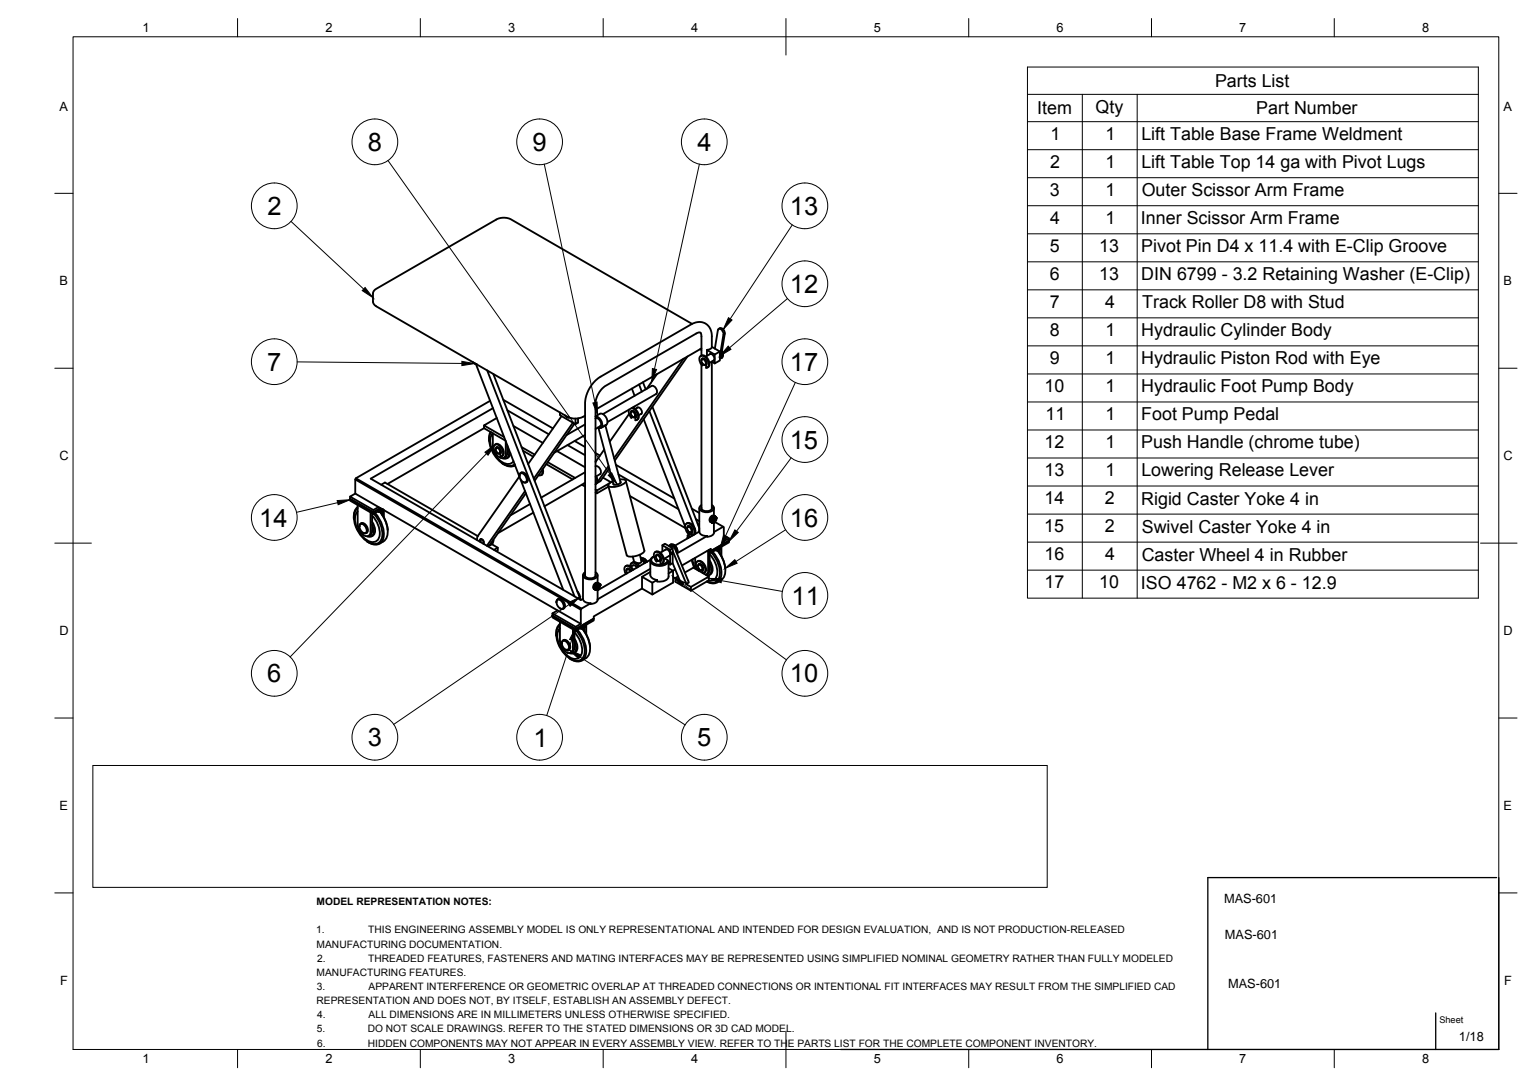
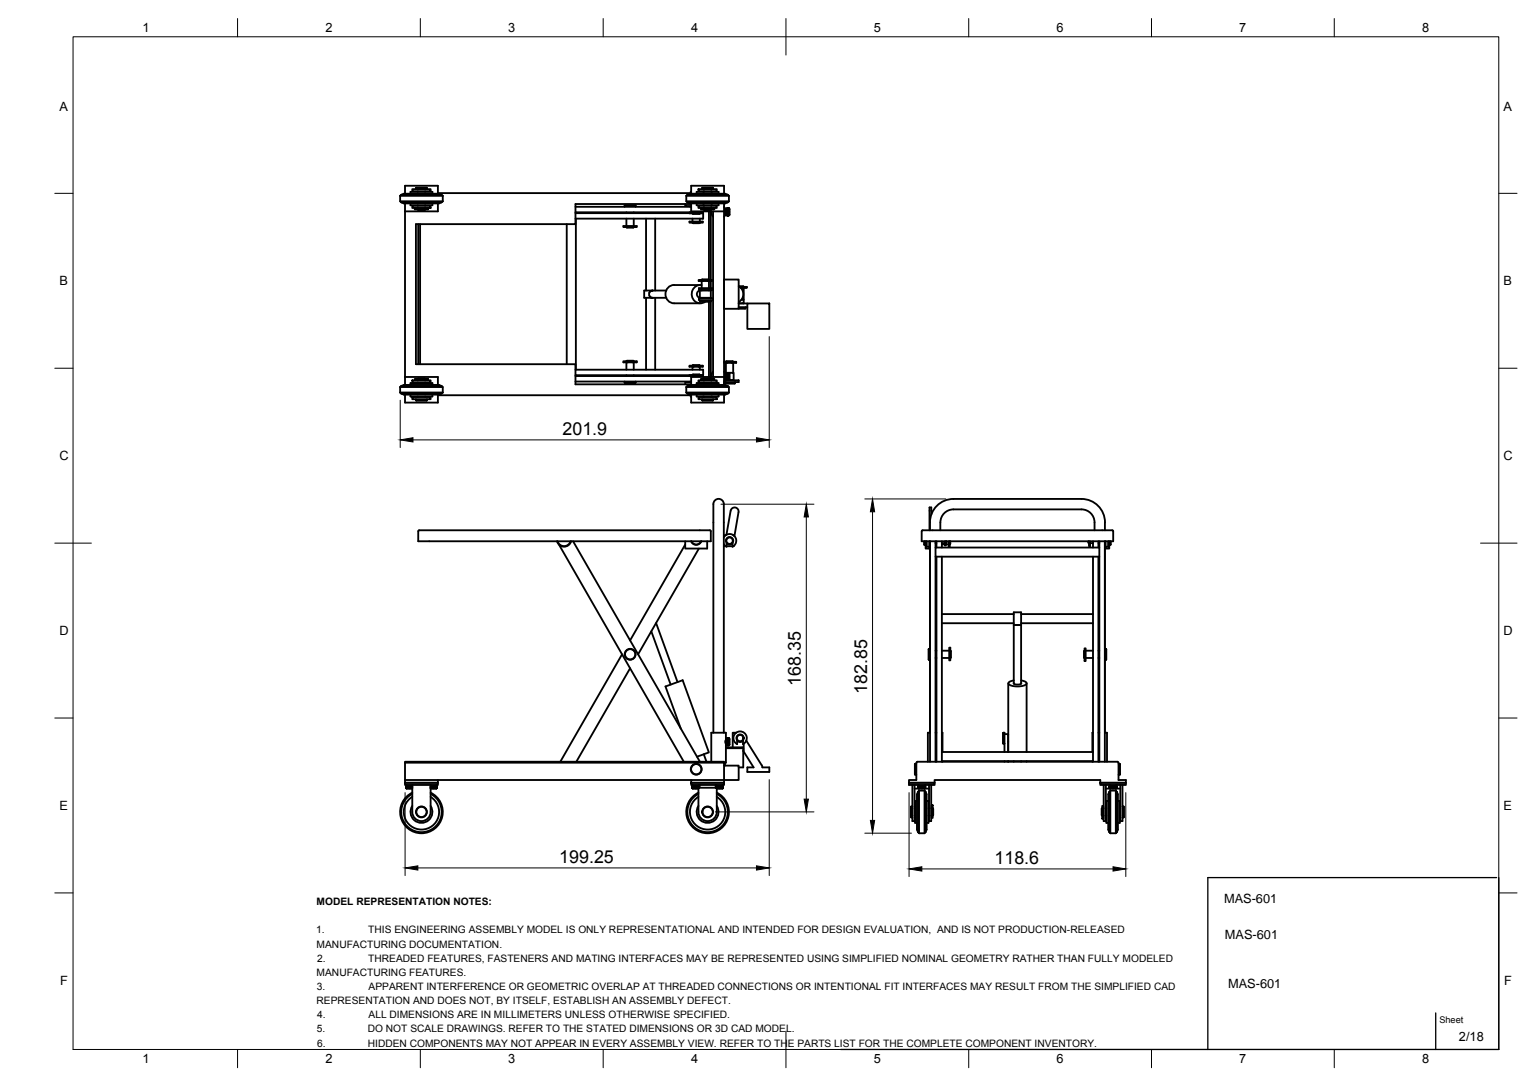
ISO-10303-21;
HEADER;
FILE_DESCRIPTION((''),'2;1');
FILE_NAME('MAS-601','2026-10-06T07:37:42+05:00',(''),(''),'','','');
FILE_SCHEMA (('AUTOMOTIVE_DESIGN { 1 0 10303 214 3 1 1 }'));
ENDSEC;
DATA;
#10 = MECHANICAL_DESIGN_GEOMETRIC_PRESENTATION_REPRESENTATION('',(#373,#374,
#375,#376,#377,#378,#379,#380,#381,#382,#383,#384,#385,#386,#387,#388,#389),
#18757) ;
#11 = ITEM_DEFINED_TRANSFORMATION($,$,#9748,#10657) ;
#12 = ITEM_DEFINED_TRANSFORMATION($,$,#9905,#10658) ;
#13 = ITEM_DEFINED_TRANSFORMATION($,$,#9983,#10659) ;
#14 = ITEM_DEFINED_TRANSFORMATION($,$,#10025,#10660) ;
#15 = ITEM_DEFINED_TRANSFORMATION($,$,#10219,#10661) ;
#16 = ITEM_DEFINED_TRANSFORMATION($,$,#10241,#10662) ;
#17 = ITEM_DEFINED_TRANSFORMATION($,$,#10254,#10663) ;
#18 = ITEM_DEFINED_TRANSFORMATION($,$,#10070,#10664) ;
#19 = ITEM_DEFINED_TRANSFORMATION($,$,#10098,#10665) ;
#20 = ITEM_DEFINED_TRANSFORMATION($,$,#10122,#10666) ;
#21 = ITEM_DEFINED_TRANSFORMATION($,$,#10152,#10667) ;
#22 = ITEM_DEFINED_TRANSFORMATION($,$,#10171,#10668) ;
#23 = ITEM_DEFINED_TRANSFORMATION($,$,#10205,#10669) ;
#24 = ITEM_DEFINED_TRANSFORMATION($,$,#10599,#10670) ;
#25 = ITEM_DEFINED_TRANSFORMATION($,$,#10552,#10671) ;
#26 = ITEM_DEFINED_TRANSFORMATION($,$,#10632,#10672) ;
#27 = ITEM_DEFINED_TRANSFORMATION($,$,#10270,#10673) ;
#28 = ITEM_DEFINED_TRANSFORMATION($,$,#10219,#10674) ;
#29 = ITEM_DEFINED_TRANSFORMATION($,$,#10241,#10675) ;
#30 = ITEM_DEFINED_TRANSFORMATION($,$,#10219,#10676) ;
#31 = ITEM_DEFINED_TRANSFORMATION($,$,#10241,#10677) ;
#32 = ITEM_DEFINED_TRANSFORMATION($,$,#10219,#10678) ;
#33 = ITEM_DEFINED_TRANSFORMATION($,$,#10241,#10679) ;
#34 = ITEM_DEFINED_TRANSFORMATION($,$,#10219,#10680) ;
#35 = ITEM_DEFINED_TRANSFORMATION($,$,#10241,#10681) ;
#36 = ITEM_DEFINED_TRANSFORMATION($,$,#10219,#10682) ;
#37 = ITEM_DEFINED_TRANSFORMATION($,$,#10241,#10683) ;
#38 = ITEM_DEFINED_TRANSFORMATION($,$,#10219,#10684) ;
#39 = ITEM_DEFINED_TRANSFORMATION($,$,#10241,#10685) ;
#40 = ITEM_DEFINED_TRANSFORMATION($,$,#10219,#10686) ;
#41 = ITEM_DEFINED_TRANSFORMATION($,$,#10241,#10687) ;
#42 = ITEM_DEFINED_TRANSFORMATION($,$,#10219,#10688) ;
#43 = ITEM_DEFINED_TRANSFORMATION($,$,#10241,#10689) ;
#44 = ITEM_DEFINED_TRANSFORMATION($,$,#10219,#10690) ;
#45 = ITEM_DEFINED_TRANSFORMATION($,$,#10241,#10691) ;
#46 = ITEM_DEFINED_TRANSFORMATION($,$,#10219,#10692) ;
#47 = ITEM_DEFINED_TRANSFORMATION($,$,#10241,#10693) ;
#48 = ITEM_DEFINED_TRANSFORMATION($,$,#10219,#10694) ;
#49 = ITEM_DEFINED_TRANSFORMATION($,$,#10241,#10695) ;
#50 = ITEM_DEFINED_TRANSFORMATION($,$,#10219,#10696) ;
#51 = ITEM_DEFINED_TRANSFORMATION($,$,#10241,#10697) ;
#52 = ITEM_DEFINED_TRANSFORMATION($,$,#10254,#10698) ;
#53 = ITEM_DEFINED_TRANSFORMATION($,$,#10254,#10699) ;
#54 = ITEM_DEFINED_TRANSFORMATION($,$,#10254,#10700) ;
#55 = ITEM_DEFINED_TRANSFORMATION($,$,#10270,#10701) ;
#56 = ITEM_DEFINED_TRANSFORMATION($,$,#10270,#10702) ;
#57 = ITEM_DEFINED_TRANSFORMATION($,$,#10270,#10703) ;
#58 = ITEM_DEFINED_TRANSFORMATION($,$,#10270,#10704) ;
#59 = ITEM_DEFINED_TRANSFORMATION($,$,#10270,#10705) ;
#60 = ITEM_DEFINED_TRANSFORMATION($,$,#10270,#10706) ;
#61 = ITEM_DEFINED_TRANSFORMATION($,$,#10270,#10707) ;
#62 = ITEM_DEFINED_TRANSFORMATION($,$,#10270,#10708) ;
#63 = ITEM_DEFINED_TRANSFORMATION($,$,#10270,#10709) ;
#64 = ITEM_DEFINED_TRANSFORMATION($,$,#10552,#10710) ;
#65 = ITEM_DEFINED_TRANSFORMATION($,$,#10599,#10711) ;
#66 = ITEM_DEFINED_TRANSFORMATION($,$,#10632,#10712) ;
#67 = ITEM_DEFINED_TRANSFORMATION($,$,#10632,#10713) ;
#68 = ITEM_DEFINED_TRANSFORMATION($,$,#10632,#10714) ;
#69 = (
REPRESENTATION_RELATIONSHIP($,$,#18857,#18856)
REPRESENTATION_RELATIONSHIP_WITH_TRANSFORMATION(#11)
SHAPE_REPRESENTATION_RELATIONSHIP()
) ;
#70 = (
REPRESENTATION_RELATIONSHIP($,$,#18858,#18856)
REPRESENTATION_RELATIONSHIP_WITH_TRANSFORMATION(#12)
SHAPE_REPRESENTATION_RELATIONSHIP()
) ;
#71 = (
REPRESENTATION_RELATIONSHIP($,$,#18859,#18856)
REPRESENTATION_RELATIONSHIP_WITH_TRANSFORMATION(#13)
SHAPE_REPRESENTATION_RELATIONSHIP()
) ;
#72 = (
REPRESENTATION_RELATIONSHIP($,$,#18860,#18856)
REPRESENTATION_RELATIONSHIP_WITH_TRANSFORMATION(#14)
SHAPE_REPRESENTATION_RELATIONSHIP()
) ;
#73 = (
REPRESENTATION_RELATIONSHIP($,$,#18867,#18856)
REPRESENTATION_RELATIONSHIP_WITH_TRANSFORMATION(#15)
SHAPE_REPRESENTATION_RELATIONSHIP()
) ;
#74 = (
REPRESENTATION_RELATIONSHIP($,$,#18868,#18856)
REPRESENTATION_RELATIONSHIP_WITH_TRANSFORMATION(#16)
SHAPE_REPRESENTATION_RELATIONSHIP()
) ;
#75 = (
REPRESENTATION_RELATIONSHIP($,$,#18869,#18856)
REPRESENTATION_RELATIONSHIP_WITH_TRANSFORMATION(#17)
SHAPE_REPRESENTATION_RELATIONSHIP()
) ;
#76 = (
REPRESENTATION_RELATIONSHIP($,$,#18861,#18856)
REPRESENTATION_RELATIONSHIP_WITH_TRANSFORMATION(#18)
SHAPE_REPRESENTATION_RELATIONSHIP()
) ;
#77 = (
REPRESENTATION_RELATIONSHIP($,$,#18862,#18856)
REPRESENTATION_RELATIONSHIP_WITH_TRANSFORMATION(#19)
SHAPE_REPRESENTATION_RELATIONSHIP()
) ;
#78 = (
REPRESENTATION_RELATIONSHIP($,$,#18863,#18856)
REPRESENTATION_RELATIONSHIP_WITH_TRANSFORMATION(#20)
SHAPE_REPRESENTATION_RELATIONSHIP()
) ;
#79 = (
REPRESENTATION_RELATIONSHIP($,$,#18864,#18856)
REPRESENTATION_RELATIONSHIP_WITH_TRANSFORMATION(#21)
SHAPE_REPRESENTATION_RELATIONSHIP()
) ;
#80 = (
REPRESENTATION_RELATIONSHIP($,$,#18865,#18856)
REPRESENTATION_RELATIONSHIP_WITH_TRANSFORMATION(#22)
SHAPE_REPRESENTATION_RELATIONSHIP()
) ;
#81 = (
REPRESENTATION_RELATIONSHIP($,$,#18866,#18856)
REPRESENTATION_RELATIONSHIP_WITH_TRANSFORMATION(#23)
SHAPE_REPRESENTATION_RELATIONSHIP()
) ;
#82 = (
REPRESENTATION_RELATIONSHIP($,$,#18872,#18856)
REPRESENTATION_RELATIONSHIP_WITH_TRANSFORMATION(#24)
SHAPE_REPRESENTATION_RELATIONSHIP()
) ;
#83 = (
REPRESENTATION_RELATIONSHIP($,$,#18871,#18856)
REPRESENTATION_RELATIONSHIP_WITH_TRANSFORMATION(#25)
SHAPE_REPRESENTATION_RELATIONSHIP()
) ;
#84 = (
REPRESENTATION_RELATIONSHIP($,$,#18873,#18856)
REPRESENTATION_RELATIONSHIP_WITH_TRANSFORMATION(#26)
SHAPE_REPRESENTATION_RELATIONSHIP()
) ;
#85 = (
REPRESENTATION_RELATIONSHIP($,$,#18870,#18856)
REPRESENTATION_RELATIONSHIP_WITH_TRANSFORMATION(#27)
SHAPE_REPRESENTATION_RELATIONSHIP()
) ;
#86 = (
REPRESENTATION_RELATIONSHIP($,$,#18867,#18856)
REPRESENTATION_RELATIONSHIP_WITH_TRANSFORMATION(#28)
SHAPE_REPRESENTATION_RELATIONSHIP()
) ;
#87 = (
REPRESENTATION_RELATIONSHIP($,$,#18868,#18856)
REPRESENTATION_RELATIONSHIP_WITH_TRANSFORMATION(#29)
SHAPE_REPRESENTATION_RELATIONSHIP()
) ;
#88 = (
REPRESENTATION_RELATIONSHIP($,$,#18867,#18856)
REPRESENTATION_RELATIONSHIP_WITH_TRANSFORMATION(#30)
SHAPE_REPRESENTATION_RELATIONSHIP()
) ;
#89 = (
REPRESENTATION_RELATIONSHIP($,$,#18868,#18856)
REPRESENTATION_RELATIONSHIP_WITH_TRANSFORMATION(#31)
SHAPE_REPRESENTATION_RELATIONSHIP()
) ;
#90 = (
REPRESENTATION_RELATIONSHIP($,$,#18867,#18856)
REPRESENTATION_RELATIONSHIP_WITH_TRANSFORMATION(#32)
SHAPE_REPRESENTATION_RELATIONSHIP()
) ;
#91 = (
REPRESENTATION_RELATIONSHIP($,$,#18868,#18856)
REPRESENTATION_RELATIONSHIP_WITH_TRANSFORMATION(#33)
SHAPE_REPRESENTATION_RELATIONSHIP()
) ;
#92 = (
REPRESENTATION_RELATIONSHIP($,$,#18867,#18856)
REPRESENTATION_RELATIONSHIP_WITH_TRANSFORMATION(#34)
SHAPE_REPRESENTATION_RELATIONSHIP()
) ;
#93 = (
REPRESENTATION_RELATIONSHIP($,$,#18868,#18856)
REPRESENTATION_RELATIONSHIP_WITH_TRANSFORMATION(#35)
SHAPE_REPRESENTATION_RELATIONSHIP()
) ;
#94 = (
REPRESENTATION_RELATIONSHIP($,$,#18867,#18856)
REPRESENTATION_RELATIONSHIP_WITH_TRANSFORMATION(#36)
SHAPE_REPRESENTATION_RELATIONSHIP()
) ;
#95 = (
REPRESENTATION_RELATIONSHIP($,$,#18868,#18856)
REPRESENTATION_RELATIONSHIP_WITH_TRANSFORMATION(#37)
SHAPE_REPRESENTATION_RELATIONSHIP()
) ;
#96 = (
REPRESENTATION_RELATIONSHIP($,$,#18867,#18856)
REPRESENTATION_RELATIONSHIP_WITH_TRANSFORMATION(#38)
SHAPE_REPRESENTATION_RELATIONSHIP()
) ;
#97 = (
REPRESENTATION_RELATIONSHIP($,$,#18868,#18856)
REPRESENTATION_RELATIONSHIP_WITH_TRANSFORMATION(#39)
SHAPE_REPRESENTATION_RELATIONSHIP()
) ;
#98 = (
REPRESENTATION_RELATIONSHIP($,$,#18867,#18856)
REPRESENTATION_RELATIONSHIP_WITH_TRANSFORMATION(#40)
SHAPE_REPRESENTATION_RELATIONSHIP()
) ;
#99 = (
REPRESENTATION_RELATIONSHIP($,$,#18868,#18856)
REPRESENTATION_RELATIONSHIP_WITH_TRANSFORMATION(#41)
SHAPE_REPRESENTATION_RELATIONSHIP()
) ;
#100 = (
REPRESENTATION_RELATIONSHIP($,$,#18867,#18856)
REPRESENTATION_RELATIONSHIP_WITH_TRANSFORMATION(#42)
SHAPE_REPRESENTATION_RELATIONSHIP()
) ;
#101 = (
REPRESENTATION_RELATIONSHIP($,$,#18868,#18856)
REPRESENTATION_RELATIONSHIP_WITH_TRANSFORMATION(#43)
SHAPE_REPRESENTATION_RELATIONSHIP()
) ;
#102 = (
REPRESENTATION_RELATIONSHIP($,$,#18867,#18856)
REPRESENTATION_RELATIONSHIP_WITH_TRANSFORMATION(#44)
SHAPE_REPRESENTATION_RELATIONSHIP()
) ;
#103 = (
REPRESENTATION_RELATIONSHIP($,$,#18868,#18856)
REPRESENTATION_RELATIONSHIP_WITH_TRANSFORMATION(#45)
SHAPE_REPRESENTATION_RELATIONSHIP()
) ;
#104 = (
REPRESENTATION_RELATIONSHIP($,$,#18867,#18856)
REPRESENTATION_RELATIONSHIP_WITH_TRANSFORMATION(#46)
SHAPE_REPRESENTATION_RELATIONSHIP()
) ;
#105 = (
REPRESENTATION_RELATIONSHIP($,$,#18868,#18856)
REPRESENTATION_RELATIONSHIP_WITH_TRANSFORMATION(#47)
SHAPE_REPRESENTATION_RELATIONSHIP()
) ;
#106 = (
REPRESENTATION_RELATIONSHIP($,$,#18867,#18856)
REPRESENTATION_RELATIONSHIP_WITH_TRANSFORMATION(#48)
SHAPE_REPRESENTATION_RELATIONSHIP()
) ;
#107 = (
REPRESENTATION_RELATIONSHIP($,$,#18868,#18856)
REPRESENTATION_RELATIONSHIP_WITH_TRANSFORMATION(#49)
SHAPE_REPRESENTATION_RELATIONSHIP()
) ;
#108 = (
REPRESENTATION_RELATIONSHIP($,$,#18867,#18856)
REPRESENTATION_RELATIONSHIP_WITH_TRANSFORMATION(#50)
SHAPE_REPRESENTATION_RELATIONSHIP()
) ;
#109 = (
REPRESENTATION_RELATIONSHIP($,$,#18868,#18856)
REPRESENTATION_RELATIONSHIP_WITH_TRANSFORMATION(#51)
SHAPE_REPRESENTATION_RELATIONSHIP()
) ;
#110 = (
REPRESENTATION_RELATIONSHIP($,$,#18869,#18856)
REPRESENTATION_RELATIONSHIP_WITH_TRANSFORMATION(#52)
SHAPE_REPRESENTATION_RELATIONSHIP()
) ;
#111 = (
REPRESENTATION_RELATIONSHIP($,$,#18869,#18856)
REPRESENTATION_RELATIONSHIP_WITH_TRANSFORMATION(#53)
SHAPE_REPRESENTATION_RELATIONSHIP()
) ;
#112 = (
REPRESENTATION_RELATIONSHIP($,$,#18869,#18856)
REPRESENTATION_RELATIONSHIP_WITH_TRANSFORMATION(#54)
SHAPE_REPRESENTATION_RELATIONSHIP()
) ;
#113 = (
REPRESENTATION_RELATIONSHIP($,$,#18870,#18856)
REPRESENTATION_RELATIONSHIP_WITH_TRANSFORMATION(#55)
SHAPE_REPRESENTATION_RELATIONSHIP()
) ;
#114 = (
REPRESENTATION_RELATIONSHIP($,$,#18870,#18856)
REPRESENTATION_RELATIONSHIP_WITH_TRANSFORMATION(#56)
SHAPE_REPRESENTATION_RELATIONSHIP()
) ;
#115 = (
REPRESENTATION_RELATIONSHIP($,$,#18870,#18856)
REPRESENTATION_RELATIONSHIP_WITH_TRANSFORMATION(#57)
SHAPE_REPRESENTATION_RELATIONSHIP()
) ;
#116 = (
REPRESENTATION_RELATIONSHIP($,$,#18870,#18856)
REPRESENTATION_RELATIONSHIP_WITH_TRANSFORMATION(#58)
SHAPE_REPRESENTATION_RELATIONSHIP()
) ;
#117 = (
REPRESENTATION_RELATIONSHIP($,$,#18870,#18856)
REPRESENTATION_RELATIONSHIP_WITH_TRANSFORMATION(#59)
SHAPE_REPRESENTATION_RELATIONSHIP()
) ;
#118 = (
REPRESENTATION_RELATIONSHIP($,$,#18870,#18856)
REPRESENTATION_RELATIONSHIP_WITH_TRANSFORMATION(#60)
SHAPE_REPRESENTATION_RELATIONSHIP()
) ;
#119 = (
REPRESENTATION_RELATIONSHIP($,$,#18870,#18856)
REPRESENTATION_RELATIONSHIP_WITH_TRANSFORMATION(#61)
SHAPE_REPRESENTATION_RELATIONSHIP()
) ;
#120 = (
REPRESENTATION_RELATIONSHIP($,$,#18870,#18856)
REPRESENTATION_RELATIONSHIP_WITH_TRANSFORMATION(#62)
SHAPE_REPRESENTATION_RELATIONSHIP()
) ;
#121 = (
REPRESENTATION_RELATIONSHIP($,$,#18870,#18856)
REPRESENTATION_RELATIONSHIP_WITH_TRANSFORMATION(#63)
SHAPE_REPRESENTATION_RELATIONSHIP()
) ;
#122 = (
REPRESENTATION_RELATIONSHIP($,$,#18871,#18856)
REPRESENTATION_RELATIONSHIP_WITH_TRANSFORMATION(#64)
SHAPE_REPRESENTATION_RELATIONSHIP()
) ;
#123 = (
REPRESENTATION_RELATIONSHIP($,$,#18872,#18856)
REPRESENTATION_RELATIONSHIP_WITH_TRANSFORMATION(#65)
SHAPE_REPRESENTATION_RELATIONSHIP()
) ;
#124 = (
REPRESENTATION_RELATIONSHIP($,$,#18873,#18856)
REPRESENTATION_RELATIONSHIP_WITH_TRANSFORMATION(#66)
SHAPE_REPRESENTATION_RELATIONSHIP()
) ;
#125 = (
REPRESENTATION_RELATIONSHIP($,$,#18873,#18856)
REPRESENTATION_RELATIONSHIP_WITH_TRANSFORMATION(#67)
SHAPE_REPRESENTATION_RELATIONSHIP()
) ;
#126 = (
REPRESENTATION_RELATIONSHIP($,$,#18873,#18856)
REPRESENTATION_RELATIONSHIP_WITH_TRANSFORMATION(#68)
SHAPE_REPRESENTATION_RELATIONSHIP()
) ;
#127 = CONTEXT_DEPENDENT_SHAPE_REPRESENTATION(#69,#18798) ;
#128 = CONTEXT_DEPENDENT_SHAPE_REPRESENTATION(#70,#18799) ;
#129 = CONTEXT_DEPENDENT_SHAPE_REPRESENTATION(#71,#18800) ;
#130 = CONTEXT_DEPENDENT_SHAPE_REPRESENTATION(#72,#18801) ;
#131 = CONTEXT_DEPENDENT_SHAPE_REPRESENTATION(#73,#18802) ;
#132 = CONTEXT_DEPENDENT_SHAPE_REPRESENTATION(#74,#18803) ;
#133 = CONTEXT_DEPENDENT_SHAPE_REPRESENTATION(#75,#18804) ;
#134 = CONTEXT_DEPENDENT_SHAPE_REPRESENTATION(#76,#18805) ;
#135 = CONTEXT_DEPENDENT_SHAPE_REPRESENTATION(#77,#18806) ;
#136 = CONTEXT_DEPENDENT_SHAPE_REPRESENTATION(#78,#18807) ;
#137 = CONTEXT_DEPENDENT_SHAPE_REPRESENTATION(#79,#18808) ;
#138 = CONTEXT_DEPENDENT_SHAPE_REPRESENTATION(#80,#18809) ;
#139 = CONTEXT_DEPENDENT_SHAPE_REPRESENTATION(#81,#18810) ;
#140 = CONTEXT_DEPENDENT_SHAPE_REPRESENTATION(#82,#18811) ;
#141 = CONTEXT_DEPENDENT_SHAPE_REPRESENTATION(#83,#18812) ;
#142 = CONTEXT_DEPENDENT_SHAPE_REPRESENTATION(#84,#18813) ;
#143 = CONTEXT_DEPENDENT_SHAPE_REPRESENTATION(#85,#18814) ;
#144 = CONTEXT_DEPENDENT_SHAPE_REPRESENTATION(#86,#18815) ;
#145 = CONTEXT_DEPENDENT_SHAPE_REPRESENTATION(#87,#18816) ;
#146 = CONTEXT_DEPENDENT_SHAPE_REPRESENTATION(#88,#18817) ;
#147 = CONTEXT_DEPENDENT_SHAPE_REPRESENTATION(#89,#18818) ;
#148 = CONTEXT_DEPENDENT_SHAPE_REPRESENTATION(#90,#18819) ;
#149 = CONTEXT_DEPENDENT_SHAPE_REPRESENTATION(#91,#18820) ;
#150 = CONTEXT_DEPENDENT_SHAPE_REPRESENTATION(#92,#18821) ;
#151 = CONTEXT_DEPENDENT_SHAPE_REPRESENTATION(#93,#18822) ;
#152 = CONTEXT_DEPENDENT_SHAPE_REPRESENTATION(#94,#18823) ;
#153 = CONTEXT_DEPENDENT_SHAPE_REPRESENTATION(#95,#18824) ;
#154 = CONTEXT_DEPENDENT_SHAPE_REPRESENTATION(#96,#18825) ;
#155 = CONTEXT_DEPENDENT_SHAPE_REPRESENTATION(#97,#18826) ;
#156 = CONTEXT_DEPENDENT_SHAPE_REPRESENTATION(#98,#18827) ;
#157 = CONTEXT_DEPENDENT_SHAPE_REPRESENTATION(#99,#18828) ;
#158 = CONTEXT_DEPENDENT_SHAPE_REPRESENTATION(#100,#18829) ;
#159 = CONTEXT_DEPENDENT_SHAPE_REPRESENTATION(#101,#18830) ;
#160 = CONTEXT_DEPENDENT_SHAPE_REPRESENTATION(#102,#18831) ;
#161 = CONTEXT_DEPENDENT_SHAPE_REPRESENTATION(#103,#18832) ;
#162 = CONTEXT_DEPENDENT_SHAPE_REPRESENTATION(#104,#18833) ;
#163 = CONTEXT_DEPENDENT_SHAPE_REPRESENTATION(#105,#18834) ;
#164 = CONTEXT_DEPENDENT_SHAPE_REPRESENTATION(#106,#18835) ;
#165 = CONTEXT_DEPENDENT_SHAPE_REPRESENTATION(#107,#18836) ;
#166 = CONTEXT_DEPENDENT_SHAPE_REPRESENTATION(#108,#18837) ;
#167 = CONTEXT_DEPENDENT_SHAPE_REPRESENTATION(#109,#18838) ;
#168 = CONTEXT_DEPENDENT_SHAPE_REPRESENTATION(#110,#18839) ;
#169 = CONTEXT_DEPENDENT_SHAPE_REPRESENTATION(#111,#18840) ;
#170 = CONTEXT_DEPENDENT_SHAPE_REPRESENTATION(#112,#18841) ;
#171 = CONTEXT_DEPENDENT_SHAPE_REPRESENTATION(#113,#18842) ;
#172 = CONTEXT_DEPENDENT_SHAPE_REPRESENTATION(#114,#18843) ;
#173 = CONTEXT_DEPENDENT_SHAPE_REPRESENTATION(#115,#18844) ;
#174 = CONTEXT_DEPENDENT_SHAPE_REPRESENTATION(#116,#18845) ;
#175 = CONTEXT_DEPENDENT_SHAPE_REPRESENTATION(#117,#18846) ;
#176 = CONTEXT_DEPENDENT_SHAPE_REPRESENTATION(#118,#18847) ;
#177 = CONTEXT_DEPENDENT_SHAPE_REPRESENTATION(#119,#18848) ;
#178 = CONTEXT_DEPENDENT_SHAPE_REPRESENTATION(#120,#18849) ;
#179 = CONTEXT_DEPENDENT_SHAPE_REPRESENTATION(#121,#18850) ;
#180 = CONTEXT_DEPENDENT_SHAPE_REPRESENTATION(#122,#18851) ;
#181 = CONTEXT_DEPENDENT_SHAPE_REPRESENTATION(#123,#18852) ;
#182 = CONTEXT_DEPENDENT_SHAPE_REPRESENTATION(#124,#18853) ;
#183 = CONTEXT_DEPENDENT_SHAPE_REPRESENTATION(#125,#18854) ;
#184 = CONTEXT_DEPENDENT_SHAPE_REPRESENTATION(#126,#18855) ;
#185 = NEXT_ASSEMBLY_USAGE_OCCURRENCE('Lift Table Base Frame Weldment:1',
'Lift Table Base Frame Weldment:1','Lift Table Base Frame Weldment:1',#18875,
#18876,'Lift Table Base Frame Weldment:1') ;
#186 = NEXT_ASSEMBLY_USAGE_OCCURRENCE(
'Lift Table Top 14 ga with Pivot Lugs:1',
'Lift Table Top 14 ga with Pivot Lugs:1',
'Lift Table Top 14 ga with Pivot Lugs:1',#18875,#18877,
'Lift Table Top 14 ga with Pivot Lugs:1') ;
#187 = NEXT_ASSEMBLY_USAGE_OCCURRENCE('Outer Scissor Arm Frame:1',
'Outer Scissor Arm Frame:1','Outer Scissor Arm Frame:1',#18875,#18878,
'Outer Scissor Arm Frame:1') ;
#188 = NEXT_ASSEMBLY_USAGE_OCCURRENCE('Inner Scissor Arm Frame:1',
'Inner Scissor Arm Frame:1','Inner Scissor Arm Frame:1',#18875,#18879,
'Inner Scissor Arm Frame:1') ;
#189 = NEXT_ASSEMBLY_USAGE_OCCURRENCE(
'Pivot Pin D4 x 11.4 with E-Clip Groove:1',
'Pivot Pin D4 x 11.4 with E-Clip Groove:1',
'Pivot Pin D4 x 11.4 with E-Clip Groove:1',#18875,#18886,
'Pivot Pin D4 x 11.4 with E-Clip Groove:1') ;
#190 = NEXT_ASSEMBLY_USAGE_OCCURRENCE(
'DIN 6799 - 3.2 Retaining Washer (E-Clip):1',
'DIN 6799 - 3.2 Retaining Washer (E-Clip):1',
'DIN 6799 - 3.2 Retaining Washer (E-Clip):1',#18875,#18887,
'DIN 6799 - 3.2 Retaining Washer (E-Clip):1') ;
#191 = NEXT_ASSEMBLY_USAGE_OCCURRENCE('Track Roller D8 with Stud:1',
'Track Roller D8 with Stud:1','Track Roller D8 with Stud:1',#18875,#18888,
'Track Roller D8 with Stud:1') ;
#192 = NEXT_ASSEMBLY_USAGE_OCCURRENCE('Hydraulic Cylinder Body:1',
'Hydraulic Cylinder Body:1','Hydraulic Cylinder Body:1',#18875,#18880,
'Hydraulic Cylinder Body:1') ;
#193 = NEXT_ASSEMBLY_USAGE_OCCURRENCE('Hydraulic Piston Rod with Eye:1',
'Hydraulic Piston Rod with Eye:1','Hydraulic Piston Rod with Eye:1',#18875,
#18881,'Hydraulic Piston Rod with Eye:1') ;
#194 = NEXT_ASSEMBLY_USAGE_OCCURRENCE('Hydraulic Foot Pump Body:1',
'Hydraulic Foot Pump Body:1','Hydraulic Foot Pump Body:1',#18875,#18882,
'Hydraulic Foot Pump Body:1') ;
#195 = NEXT_ASSEMBLY_USAGE_OCCURRENCE('Foot Pump Pedal:1',
'Foot Pump Pedal:1','Foot Pump Pedal:1',#18875,#18883,
'Foot Pump Pedal:1') ;
#196 = NEXT_ASSEMBLY_USAGE_OCCURRENCE('Push Handle (chrome tube):1',
'Push Handle (chrome tube):1','Push Handle (chrome tube):1',#18875,#18884,
'Push Handle (chrome tube):1') ;
#197 = NEXT_ASSEMBLY_USAGE_OCCURRENCE('Lowering Release Lever:1',
'Lowering Release Lever:1','Lowering Release Lever:1',#18875,#18885,
'Lowering Release Lever:1') ;
#198 = NEXT_ASSEMBLY_USAGE_OCCURRENCE('Rigid Caster Yoke 4 in:1',
'Rigid Caster Yoke 4 in:1','Rigid Caster Yoke 4 in:1',#18875,#18891,
'Rigid Caster Yoke 4 in:1') ;
#199 = NEXT_ASSEMBLY_USAGE_OCCURRENCE('Swivel Caster Yoke 4 in:1',
'Swivel Caster Yoke 4 in:1','Swivel Caster Yoke 4 in:1',#18875,#18890,
'Swivel Caster Yoke 4 in:1') ;
#200 = NEXT_ASSEMBLY_USAGE_OCCURRENCE('Caster Wheel 4 in Rubber:1',
'Caster Wheel 4 in Rubber:1','Caster Wheel 4 in Rubber:1',#18875,#18892,
'Caster Wheel 4 in Rubber:1') ;
#201 = NEXT_ASSEMBLY_USAGE_OCCURRENCE('ISO 4762 - M2 x 6 - 12.9:1',
'ISO 4762 - M2 x 6 - 12.9:1','ISO 4762 - M2 x 6 - 12.9:1',#18875,#18889,
'ISO 4762 - M2 x 6 - 12.9:1') ;
#202 = NEXT_ASSEMBLY_USAGE_OCCURRENCE(
'Pivot Pin D4 x 11.4 with E-Clip Groove:2',
'Pivot Pin D4 x 11.4 with E-Clip Groove:2',
'Pivot Pin D4 x 11.4 with E-Clip Groove:2',#18875,#18886,
'Pivot Pin D4 x 11.4 with E-Clip Groove:2') ;
#203 = NEXT_ASSEMBLY_USAGE_OCCURRENCE(
'DIN 6799 - 3.2 Retaining Washer (E-Clip):2',
'DIN 6799 - 3.2 Retaining Washer (E-Clip):2',
'DIN 6799 - 3.2 Retaining Washer (E-Clip):2',#18875,#18887,
'DIN 6799 - 3.2 Retaining Washer (E-Clip):2') ;
#204 = NEXT_ASSEMBLY_USAGE_OCCURRENCE(
'Pivot Pin D4 x 11.4 with E-Clip Groove:3',
'Pivot Pin D4 x 11.4 with E-Clip Groove:3',
'Pivot Pin D4 x 11.4 with E-Clip Groove:3',#18875,#18886,
'Pivot Pin D4 x 11.4 with E-Clip Groove:3') ;
#205 = NEXT_ASSEMBLY_USAGE_OCCURRENCE(
'DIN 6799 - 3.2 Retaining Washer (E-Clip):3',
'DIN 6799 - 3.2 Retaining Washer (E-Clip):3',
'DIN 6799 - 3.2 Retaining Washer (E-Clip):3',#18875,#18887,
'DIN 6799 - 3.2 Retaining Washer (E-Clip):3') ;
#206 = NEXT_ASSEMBLY_USAGE_OCCURRENCE(
'Pivot Pin D4 x 11.4 with E-Clip Groove:4',
'Pivot Pin D4 x 11.4 with E-Clip Groove:4',
'Pivot Pin D4 x 11.4 with E-Clip Groove:4',#18875,#18886,
'Pivot Pin D4 x 11.4 with E-Clip Groove:4') ;
#207 = NEXT_ASSEMBLY_USAGE_OCCURRENCE(
'DIN 6799 - 3.2 Retaining Washer (E-Clip):4',
'DIN 6799 - 3.2 Retaining Washer (E-Clip):4',
'DIN 6799 - 3.2 Retaining Washer (E-Clip):4',#18875,#18887,
'DIN 6799 - 3.2 Retaining Washer (E-Clip):4') ;
#208 = NEXT_ASSEMBLY_USAGE_OCCURRENCE(
'Pivot Pin D4 x 11.4 with E-Clip Groove:5',
'Pivot Pin D4 x 11.4 with E-Clip Groove:5',
'Pivot Pin D4 x 11.4 with E-Clip Groove:5',#18875,#18886,
'Pivot Pin D4 x 11.4 with E-Clip Groove:5') ;
#209 = NEXT_ASSEMBLY_USAGE_OCCURRENCE(
'DIN 6799 - 3.2 Retaining Washer (E-Clip):5',
'DIN 6799 - 3.2 Retaining Washer (E-Clip):5',
'DIN 6799 - 3.2 Retaining Washer (E-Clip):5',#18875,#18887,
'DIN 6799 - 3.2 Retaining Washer (E-Clip):5') ;
#210 = NEXT_ASSEMBLY_USAGE_OCCURRENCE(
'Pivot Pin D4 x 11.4 with E-Clip Groove:6',
'Pivot Pin D4 x 11.4 with E-Clip Groove:6',
'Pivot Pin D4 x 11.4 with E-Clip Groove:6',#18875,#18886,
'Pivot Pin D4 x 11.4 with E-Clip Groove:6') ;
#211 = NEXT_ASSEMBLY_USAGE_OCCURRENCE(
'DIN 6799 - 3.2 Retaining Washer (E-Clip):6',
'DIN 6799 - 3.2 Retaining Washer (E-Clip):6',
'DIN 6799 - 3.2 Retaining Washer (E-Clip):6',#18875,#18887,
'DIN 6799 - 3.2 Retaining Washer (E-Clip):6') ;
#212 = NEXT_ASSEMBLY_USAGE_OCCURRENCE(
'Pivot Pin D4 x 11.4 with E-Clip Groove:7',
'Pivot Pin D4 x 11.4 with E-Clip Groove:7',
'Pivot Pin D4 x 11.4 with E-Clip Groove:7',#18875,#18886,
'Pivot Pin D4 x 11.4 with E-Clip Groove:7') ;
#213 = NEXT_ASSEMBLY_USAGE_OCCURRENCE(
'DIN 6799 - 3.2 Retaining Washer (E-Clip):7',
'DIN 6799 - 3.2 Retaining Washer (E-Clip):7',
'DIN 6799 - 3.2 Retaining Washer (E-Clip):7',#18875,#18887,
'DIN 6799 - 3.2 Retaining Washer (E-Clip):7') ;
#214 = NEXT_ASSEMBLY_USAGE_OCCURRENCE(
'Pivot Pin D4 x 11.4 with E-Clip Groove:8',
'Pivot Pin D4 x 11.4 with E-Clip Groove:8',
'Pivot Pin D4 x 11.4 with E-Clip Groove:8',#18875,#18886,
'Pivot Pin D4 x 11.4 with E-Clip Groove:8') ;
#215 = NEXT_ASSEMBLY_USAGE_OCCURRENCE(
'DIN 6799 - 3.2 Retaining Washer (E-Clip):8',
'DIN 6799 - 3.2 Retaining Washer (E-Clip):8',
'DIN 6799 - 3.2 Retaining Washer (E-Clip):8',#18875,#18887,
'DIN 6799 - 3.2 Retaining Washer (E-Clip):8') ;
#216 = NEXT_ASSEMBLY_USAGE_OCCURRENCE(
'Pivot Pin D4 x 11.4 with E-Clip Groove:9',
'Pivot Pin D4 x 11.4 with E-Clip Groove:9',
'Pivot Pin D4 x 11.4 with E-Clip Groove:9',#18875,#18886,
'Pivot Pin D4 x 11.4 with E-Clip Groove:9') ;
#217 = NEXT_ASSEMBLY_USAGE_OCCURRENCE(
'DIN 6799 - 3.2 Retaining Washer (E-Clip):9',
'DIN 6799 - 3.2 Retaining Washer (E-Clip):9',
'DIN 6799 - 3.2 Retaining Washer (E-Clip):9',#18875,#18887,
'DIN 6799 - 3.2 Retaining Washer (E-Clip):9') ;
#218 = NEXT_ASSEMBLY_USAGE_OCCURRENCE(
'Pivot Pin D4 x 11.4 with E-Clip Groove:10',
'Pivot Pin D4 x 11.4 with E-Clip Groove:10',
'Pivot Pin D4 x 11.4 with E-Clip Groove:10',#18875,#18886,
'Pivot Pin D4 x 11.4 with E-Clip Groove:10') ;
#219 = NEXT_ASSEMBLY_USAGE_OCCURRENCE(
'DIN 6799 - 3.2 Retaining Washer (E-Clip):10',
'DIN 6799 - 3.2 Retaining Washer (E-Clip):10',
'DIN 6799 - 3.2 Retaining Washer (E-Clip):10',#18875,#18887,
'DIN 6799 - 3.2 Retaining Washer (E-Clip):10') ;
#220 = NEXT_ASSEMBLY_USAGE_OCCURRENCE(
'Pivot Pin D4 x 11.4 with E-Clip Groove:11',
'Pivot Pin D4 x 11.4 with E-Clip Groove:11',
'Pivot Pin D4 x 11.4 with E-Clip Groove:11',#18875,#18886,
'Pivot Pin D4 x 11.4 with E-Clip Groove:11') ;
#221 = NEXT_ASSEMBLY_USAGE_OCCURRENCE(
'DIN 6799 - 3.2 Retaining Washer (E-Clip):11',
'DIN 6799 - 3.2 Retaining Washer (E-Clip):11',
'DIN 6799 - 3.2 Retaining Washer (E-Clip):11',#18875,#18887,
'DIN 6799 - 3.2 Retaining Washer (E-Clip):11') ;
#222 = NEXT_ASSEMBLY_USAGE_OCCURRENCE(
'Pivot Pin D4 x 11.4 with E-Clip Groove:12',
'Pivot Pin D4 x 11.4 with E-Clip Groove:12',
'Pivot Pin D4 x 11.4 with E-Clip Groove:12',#18875,#18886,
'Pivot Pin D4 x 11.4 with E-Clip Groove:12') ;
#223 = NEXT_ASSEMBLY_USAGE_OCCURRENCE(
'DIN 6799 - 3.2 Retaining Washer (E-Clip):12',
'DIN 6799 - 3.2 Retaining Washer (E-Clip):12',
'DIN 6799 - 3.2 Retaining Washer (E-Clip):12',#18875,#18887,
'DIN 6799 - 3.2 Retaining Washer (E-Clip):12') ;
#224 = NEXT_ASSEMBLY_USAGE_OCCURRENCE(
'Pivot Pin D4 x 11.4 with E-Clip Groove:13',
'Pivot Pin D4 x 11.4 with E-Clip Groove:13',
'Pivot Pin D4 x 11.4 with E-Clip Groove:13',#18875,#18886,
'Pivot Pin D4 x 11.4 with E-Clip Groove:13') ;
#225 = NEXT_ASSEMBLY_USAGE_OCCURRENCE(
'DIN 6799 - 3.2 Retaining Washer (E-Clip):13',
'DIN 6799 - 3.2 Retaining Washer (E-Clip):13',
'DIN 6799 - 3.2 Retaining Washer (E-Clip):13',#18875,#18887,
'DIN 6799 - 3.2 Retaining Washer (E-Clip):13') ;
#226 = NEXT_ASSEMBLY_USAGE_OCCURRENCE('Track Roller D8 with Stud:2',
'Track Roller D8 with Stud:2','Track Roller D8 with Stud:2',#18875,#18888,
'Track Roller D8 with Stud:2') ;
#227 = NEXT_ASSEMBLY_USAGE_OCCURRENCE('Track Roller D8 with Stud:3',
'Track Roller D8 with Stud:3','Track Roller D8 with Stud:3',#18875,#18888,
'Track Roller D8 with Stud:3') ;
#228 = NEXT_ASSEMBLY_USAGE_OCCURRENCE('Track Roller D8 with Stud:4',
'Track Roller D8 with Stud:4','Track Roller D8 with Stud:4',#18875,#18888,
'Track Roller D8 with Stud:4') ;
#229 = NEXT_ASSEMBLY_USAGE_OCCURRENCE('ISO 4762 - M2 x 6 - 12.9:2',
'ISO 4762 - M2 x 6 - 12.9:2','ISO 4762 - M2 x 6 - 12.9:2',#18875,#18889,
'ISO 4762 - M2 x 6 - 12.9:2') ;
#230 = NEXT_ASSEMBLY_USAGE_OCCURRENCE('ISO 4762 - M2 x 6 - 12.9:3',
'ISO 4762 - M2 x 6 - 12.9:3','ISO 4762 - M2 x 6 - 12.9:3',#18875,#18889,
'ISO 4762 - M2 x 6 - 12.9:3') ;
#231 = NEXT_ASSEMBLY_USAGE_OCCURRENCE('ISO 4762 - M2 x 6 - 12.9:4',
'ISO 4762 - M2 x 6 - 12.9:4','ISO 4762 - M2 x 6 - 12.9:4',#18875,#18889,
'ISO 4762 - M2 x 6 - 12.9:4') ;
#232 = NEXT_ASSEMBLY_USAGE_OCCURRENCE('ISO 4762 - M2 x 6 - 12.9:5',
'ISO 4762 - M2 x 6 - 12.9:5','ISO 4762 - M2 x 6 - 12.9:5',#18875,#18889,
'ISO 4762 - M2 x 6 - 12.9:5') ;
#233 = NEXT_ASSEMBLY_USAGE_OCCURRENCE('ISO 4762 - M2 x 6 - 12.9:6',
'ISO 4762 - M2 x 6 - 12.9:6','ISO 4762 - M2 x 6 - 12.9:6',#18875,#18889,
'ISO 4762 - M2 x 6 - 12.9:6') ;
#234 = NEXT_ASSEMBLY_USAGE_OCCURRENCE('ISO 4762 - M2 x 6 - 12.9:7',
'ISO 4762 - M2 x 6 - 12.9:7','ISO 4762 - M2 x 6 - 12.9:7',#18875,#18889,
'ISO 4762 - M2 x 6 - 12.9:7') ;
#235 = NEXT_ASSEMBLY_USAGE_OCCURRENCE('ISO 4762 - M2 x 6 - 12.9:8',
'ISO 4762 - M2 x 6 - 12.9:8','ISO 4762 - M2 x 6 - 12.9:8',#18875,#18889,
'ISO 4762 - M2 x 6 - 12.9:8') ;
#236 = NEXT_ASSEMBLY_USAGE_OCCURRENCE('ISO 4762 - M2 x 6 - 12.9:9',
'ISO 4762 - M2 x 6 - 12.9:9','ISO 4762 - M2 x 6 - 12.9:9',#18875,#18889,
'ISO 4762 - M2 x 6 - 12.9:9') ;
#237 = NEXT_ASSEMBLY_USAGE_OCCURRENCE('ISO 4762 - M2 x 6 - 12.9:10',
'ISO 4762 - M2 x 6 - 12.9:10','ISO 4762 - M2 x 6 - 12.9:10',#18875,#18889,
'ISO 4762 - M2 x 6 - 12.9:10') ;
#238 = NEXT_ASSEMBLY_USAGE_OCCURRENCE('Swivel Caster Yoke 4 in:2',
'Swivel Caster Yoke 4 in:2','Swivel Caster Yoke 4 in:2',#18875,#18890,
'Swivel Caster Yoke 4 in:2') ;
#239 = NEXT_ASSEMBLY_USAGE_OCCURRENCE('Rigid Caster Yoke 4 in:2',
'Rigid Caster Yoke 4 in:2','Rigid Caster Yoke 4 in:2',#18875,#18891,
'Rigid Caster Yoke 4 in:2') ;
#240 = NEXT_ASSEMBLY_USAGE_OCCURRENCE('Caster Wheel 4 in Rubber:2',
'Caster Wheel 4 in Rubber:2','Caster Wheel 4 in Rubber:2',#18875,#18892,
'Caster Wheel 4 in Rubber:2') ;
#241 = NEXT_ASSEMBLY_USAGE_OCCURRENCE('Caster Wheel 4 in Rubber:3',
'Caster Wheel 4 in Rubber:3','Caster Wheel 4 in Rubber:3',#18875,#18892,
'Caster Wheel 4 in Rubber:3') ;
#242 = NEXT_ASSEMBLY_USAGE_OCCURRENCE('Caster Wheel 4 in Rubber:4',
'Caster Wheel 4 in Rubber:4','Caster Wheel 4 in Rubber:4',#18875,#18892,
'Caster Wheel 4 in Rubber:4') ;
#243 = B_SPLINE_SURFACE_WITH_KNOTS('',3,3,((#16462,#16463,#16464,#16465,#16466,
#16467,#16468,#16469,#16470,#16471,#16472,#16473,#16474,#16475,#16476,#16477,
#16478,#16479,#16480,#16481,#16482,#16483,#16484,#16485,#16486,#16487,#16488,
#16489,#16490,#16491,#16492,#16493,#16494,#16495,#16496,#16497,#16498,#16499,
#16500,#16501,#16502,#16503,#16504,#16505,#16506,#16507,#16508,#16509,#16510,
#16511,#16512,#16513,#16514,#16515,#16516,#16517,#16518,#16519,#16520,#16521,
#16522,#16523,#16524,#16525,#16526,#16527,#16528,#16529,#16530,#16531,#16532,
#16533,#16534,#16535,#16536,#16537,#16538,#16539,#16540,#16541,#16542,#16543,
#16544,#16545,#16546,#16547,#16548,#16549,#16550,#16551,#16552,#16553,#16554),
(#16555,#16556,#16557,#16558,#16559,#16560,#16561,#16562,#16563,#16564,
#16565,#16566,#16567,#16568,#16569,#16570,#16571,#16572,#16573,#16574,#16575,
#16576,#16577,#16578,#16579,#16580,#16581,#16582,#16583,#16584,#16585,#16586,
#16587,#16588,#16589,#16590,#16591,#16592,#16593,#16594,#16595,#16596,#16597,
#16598,#16599,#16600,#16601,#16602,#16603,#16604,#16605,#16606,#16607,#16608,
#16609,#16610,#16611,#16612,#16613,#16614,#16615,#16616,#16617,#16618,#16619,
#16620,#16621,#16622,#16623,#16624,#16625,#16626,#16627,#16628,#16629,#16630,
#16631,#16632,#16633,#16634,#16635,#16636,#16637,#16638,#16639,#16640,#16641,
#16642,#16643,#16644,#16645,#16646,#16647),(#16648,#16649,#16650,#16651,
#16652,#16653,#16654,#16655,#16656,#16657,#16658,#16659,#16660,#16661,#16662,
#16663,#16664,#16665,#16666,#16667,#16668,#16669,#16670,#16671,#16672,#16673,
#16674,#16675,#16676,#16677,#16678,#16679,#16680,#16681,#16682,#16683,#16684,
#16685,#16686,#16687,#16688,#16689,#16690,#16691,#16692,#16693,#16694,#16695,
#16696,#16697,#16698,#16699,#16700,#16701,#16702,#16703,#16704,#16705,#16706,
#16707,#16708,#16709,#16710,#16711,#16712,#16713,#16714,#16715,#16716,#16717,
#16718,#16719,#16720,#16721,#16722,#16723,#16724,#16725,#16726,#16727,#16728,
#16729,#16730,#16731,#16732,#16733,#16734,#16735,#16736,#16737,#16738,#16739,
#16740),(#16741,#16742,#16743,#16744,#16745,#16746,#16747,#16748,#16749,
#16750,#16751,#16752,#16753,#16754,#16755,#16756,#16757,#16758,#16759,#16760,
#16761,#16762,#16763,#16764,#16765,#16766,#16767,#16768,#16769,#16770,#16771,
#16772,#16773,#16774,#16775,#16776,#16777,#16778,#16779,#16780,#16781,#16782,
#16783,#16784,#16785,#16786,#16787,#16788,#16789,#16790,#16791,#16792,#16793,
#16794,#16795,#16796,#16797,#16798,#16799,#16800,#16801,#16802,#16803,#16804,
#16805,#16806,#16807,#16808,#16809,#16810,#16811,#16812,#16813,#16814,#16815,
#16816,#16817,#16818,#16819,#16820,#16821,#16822,#16823,#16824,#16825,#16826,
#16827,#16828,#16829,#16830,#16831,#16832,#16833)),.UNSPECIFIED.,.F.,.F.,
 .F.,(4,4),(4,1,1,1,1,1,1,1,1,1,1,1,1,1,1,1,1,1,1,1,1,1,1,1,1,1,1,1,1,1,
1,1,1,1,1,1,1,1,1,1,1,1,1,1,1,1,1,1,1,1,1,1,1,1,1,1,1,1,1,1,1,1,1,1,1,1,
1,1,1,1,1,1,1,1,1,1,1,1,1,1,1,1,1,1,1,1,1,1,1,1,4),(0.,0.026298304761587),
(8.30929135176524,9.30089868691122,10.2925060220572,11.2841133572032,12.2757206923492,
13.2673280274952,14.2589353626411,15.2505426977871,16.2421500329331,17.2337573680791,
18.2253647032251,19.2169720383711,20.2085793735171,21.200186708663,22.191794043809,
23.183401378955,24.175008714101,25.166616049247,26.158223384393,27.149830719539,
28.1414380546849,29.1330453898309,30.1246527249769,31.1162600601229,32.1078673952689,
33.0994747304149,34.0910820655609,35.0826894007068,36.0742967358528,37.0659040709988,
38.0575114061448,39.0491187412908,40.0407260764368,41.0323334115828,42.0239407467287,
43.0155480818747,44.0071554170207,44.9987627521667,45.9903700873127,46.9819774224587,
47.9735847576047,48.9651920927506,49.9567994278966,50.9484067630426,51.9400140981886,
52.9316214333346,53.9232287684806,54.9148361036265,55.9064434387725,56.8980507739185,
57.8896581090645,58.8812654442105,59.8728727793565,60.8644801145025,61.8560874496484,
62.8476947847944,63.8393021199404,64.8309094550864,65.8225167902324,66.8141241253784,
67.8057314605244,68.7973387956703,69.7889461308163,70.7805534659623,71.7721608011083,
72.7637681362543,73.7553754714003,74.7469828065463,75.7385901416922,76.7301974768382,
77.7218048119842,78.7134121471302,79.7050194822762,80.6966268174222,81.6882341525682,
82.6798414877141,83.6714488228601,84.6630561580061,85.6546634931521,86.6462708282981,
87.6378781634441,88.62948549859,89.621092833736,90.612700168882,91.604307504028,
92.595914839174,93.58752217432,94.579129509466,95.5707368446119,96.5623441797579,
97.5539515149039),.UNSPECIFIED.) ;
#244 = B_SPLINE_SURFACE_WITH_KNOTS('',3,3,((#17024,#17025,#17026,#17027,#17028,
#17029,#17030,#17031,#17032,#17033,#17034,#17035,#17036,#17037,#17038,#17039,
#17040,#17041,#17042,#17043,#17044,#17045,#17046,#17047,#17048,#17049,#17050,
#17051,#17052,#17053,#17054,#17055,#17056,#17057,#17058,#17059,#17060,#17061,
#17062,#17063,#17064,#17065,#17066,#17067,#17068,#17069,#17070,#17071,#17072,
#17073,#17074,#17075,#17076,#17077,#17078,#17079,#17080,#17081,#17082,#17083,
#17084,#17085,#17086,#17087,#17088,#17089,#17090,#17091,#17092,#17093,#17094,
#17095,#17096,#17097,#17098,#17099,#17100,#17101,#17102,#17103,#17104,#17105,
#17106,#17107,#17108,#17109,#17110,#17111,#17112,#17113,#17114,#17115,#17116),
(#17117,#17118,#17119,#17120,#17121,#17122,#17123,#17124,#17125,#17126,
#17127,#17128,#17129,#17130,#17131,#17132,#17133,#17134,#17135,#17136,#17137,
#17138,#17139,#17140,#17141,#17142,#17143,#17144,#17145,#17146,#17147,#17148,
#17149,#17150,#17151,#17152,#17153,#17154,#17155,#17156,#17157,#17158,#17159,
#17160,#17161,#17162,#17163,#17164,#17165,#17166,#17167,#17168,#17169,#17170,
#17171,#17172,#17173,#17174,#17175,#17176,#17177,#17178,#17179,#17180,#17181,
#17182,#17183,#17184,#17185,#17186,#17187,#17188,#17189,#17190,#17191,#17192,
#17193,#17194,#17195,#17196,#17197,#17198,#17199,#17200,#17201,#17202,#17203,
#17204,#17205,#17206,#17207,#17208,#17209),(#17210,#17211,#17212,#17213,
#17214,#17215,#17216,#17217,#17218,#17219,#17220,#17221,#17222,#17223,#17224,
#17225,#17226,#17227,#17228,#17229,#17230,#17231,#17232,#17233,#17234,#17235,
#17236,#17237,#17238,#17239,#17240,#17241,#17242,#17243,#17244,#17245,#17246,
#17247,#17248,#17249,#17250,#17251,#17252,#17253,#17254,#17255,#17256,#17257,
#17258,#17259,#17260,#17261,#17262,#17263,#17264,#17265,#17266,#17267,#17268,
#17269,#17270,#17271,#17272,#17273,#17274,#17275,#17276,#17277,#17278,#17279,
#17280,#17281,#17282,#17283,#17284,#17285,#17286,#17287,#17288,#17289,#17290,
#17291,#17292,#17293,#17294,#17295,#17296,#17297,#17298,#17299,#17300,#17301,
#17302),(#17303,#17304,#17305,#17306,#17307,#17308,#17309,#17310,#17311,
#17312,#17313,#17314,#17315,#17316,#17317,#17318,#17319,#17320,#17321,#17322,
#17323,#17324,#17325,#17326,#17327,#17328,#17329,#17330,#17331,#17332,#17333,
#17334,#17335,#17336,#17337,#17338,#17339,#17340,#17341,#17342,#17343,#17344,
#17345,#17346,#17347,#17348,#17349,#17350,#17351,#17352,#17353,#17354,#17355,
#17356,#17357,#17358,#17359,#17360,#17361,#17362,#17363,#17364,#17365,#17366,
#17367,#17368,#17369,#17370,#17371,#17372,#17373,#17374,#17375,#17376,#17377,
#17378,#17379,#17380,#17381,#17382,#17383,#17384,#17385,#17386,#17387,#17388,
#17389,#17390,#17391,#17392,#17393,#17394,#17395)),.UNSPECIFIED.,.F.,.F.,
 .F.,(4,4),(4,1,1,1,1,1,1,1,1,1,1,1,1,1,1,1,1,1,1,1,1,1,1,1,1,1,1,1,1,1,
1,1,1,1,1,1,1,1,1,1,1,1,1,1,1,1,1,1,1,1,1,1,1,1,1,1,1,1,1,1,1,1,1,1,1,1,
1,1,1,1,1,1,1,1,1,1,1,1,1,1,1,1,1,1,1,1,1,1,1,1,4),(0.,0.026298304761587),
(11.6163931973414,12.6080005324874,13.5996078676334,14.5912152027794,15.5828225379253,
16.5744298730713,17.5660372082173,18.5576445433633,19.5492518785093,20.5408592136553,
21.5324665488013,22.5240738839472,23.5156812190932,24.5072885542392,25.4988958893852,
26.4905032245312,27.4821105596772,28.4737178948232,29.4653252299691,30.4569325651151,
31.4485399002611,32.4401472354071,33.4317545705531,34.4233619056991,35.4149692408451,
36.406576575991,37.398183911137,38.389791246283,39.381398581429,40.373005916575,
41.364613251721,42.356220586867,43.3478279220129,44.3394352571589,45.3310425923049,
46.3226499274509,47.3142572625969,48.3058645977429,49.2974719328889,50.2890792680348,
51.2806866031808,52.2722939383268,53.2639012734728,54.2555086086188,55.2471159437648,
56.2387232789108,57.2303306140567,58.2219379492027,59.2135452843487,60.2051526194947,
61.1967599546407,62.1883672897867,63.1799746249327,64.1715819600786,65.1631892952246,
66.1547966303706,67.1464039655166,68.1380113006626,69.1296186358086,70.1212259709546,
71.1128333061005,72.1044406412465,73.0960479763925,74.0876553115385,75.0792626466845,
76.0708699818305,77.0624773169765,78.0540846521224,79.0456919872684,80.0372993224144,
81.0289066575604,82.0205139927064,83.0121213278524,84.0037286629984,84.9953359981443,
85.9869433332903,86.9785506684363,87.9701580035823,88.9617653387283,89.9533726738743,
90.9449800090203,91.9365873441662,92.9281946793122,93.9198020144582,94.9114093496042,
95.9030166847502,96.8946240198962,97.8862313550422,98.8778386901881,99.8694460253341,
100.86105336048),.UNSPECIFIED.) ;
#245 = (
BOUNDED_CURVE()
B_SPLINE_CURVE(2,(#14772,#14773,#14774),.UNSPECIFIED.,.F.,.F.)
B_SPLINE_CURVE_WITH_KNOTS((3,3),(0.,0.0816843221416426),.UNSPECIFIED.)
CURVE()
GEOMETRIC_REPRESENTATION_ITEM()
RATIONAL_B_SPLINE_CURVE((1.,1.00231931413628,1.))
REPRESENTATION_ITEM('')
) ;
#246 = (
BOUNDED_CURVE()
B_SPLINE_CURVE(2,(#14806,#14807,#14808),.UNSPECIFIED.,.F.,.F.)
B_SPLINE_CURVE_WITH_KNOTS((3,3),(0.,0.0711625451007686),.UNSPECIFIED.)
CURVE()
GEOMETRIC_REPRESENTATION_ITEM()
RATIONAL_B_SPLINE_CURVE((1.,1.00142359213772,1.))
REPRESENTATION_ITEM('')
) ;
#247 = (
BOUNDED_CURVE()
B_SPLINE_CURVE(2,(#17435,#17436,#17437),.UNSPECIFIED.,.F.,.F.)
B_SPLINE_CURVE_WITH_KNOTS((3,3),(0.,0.0208203041101871),.UNSPECIFIED.)
CURVE()
GEOMETRIC_REPRESENTATION_ITEM()
RATIONAL_B_SPLINE_CURVE((1.,1.00198318129131,1.00207919474364))
REPRESENTATION_ITEM('')
) ;
#248 = (
BOUNDED_CURVE()
B_SPLINE_CURVE(2,(#17441,#17442,#17443),.UNSPECIFIED.,.F.,.F.)
B_SPLINE_CURVE_WITH_KNOTS((3,3),(0.0229388536475348,0.0437591577578469),
 .UNSPECIFIED.)
CURVE()
GEOMETRIC_REPRESENTATION_ITEM()
RATIONAL_B_SPLINE_CURVE((1.00207919472777,1.00198318127619,1.))
REPRESENTATION_ITEM('')
) ;
#249 = (
BOUNDED_CURVE()
B_SPLINE_CURVE(2,(#17736,#17737,#17738),.UNSPECIFIED.,.F.,.F.)
B_SPLINE_CURVE_WITH_KNOTS((3,3),(0.,0.020820304110201),.UNSPECIFIED.)
CURVE()
GEOMETRIC_REPRESENTATION_ITEM()
RATIONAL_B_SPLINE_CURVE((1.,1.00198318127951,1.00207919473126))
REPRESENTATION_ITEM('')
) ;
#250 = (
BOUNDED_CURVE()
B_SPLINE_CURVE(2,(#17740,#17741,#17742),.UNSPECIFIED.,.F.,.F.)
B_SPLINE_CURVE_WITH_KNOTS((3,3),(0.0229388536477412,0.043759157757845),
 .UNSPECIFIED.)
CURVE()
GEOMETRIC_REPRESENTATION_ITEM()
RATIONAL_B_SPLINE_CURVE((1.00207919475953,1.00198318130646,1.))
REPRESENTATION_ITEM('')
) ;
#251 = (
BOUNDED_CURVE()
B_SPLINE_CURVE(2,(#17750,#17751,#17752),.UNSPECIFIED.,.F.,.F.)
B_SPLINE_CURVE_WITH_KNOTS((3,3),(0.0229388536475751,0.0437591577578467),
 .UNSPECIFIED.)
CURVE()
GEOMETRIC_REPRESENTATION_ITEM()
RATIONAL_B_SPLINE_CURVE((1.00207919474459,1.00198318129223,1.))
REPRESENTATION_ITEM('')
) ;
#252 = (
BOUNDED_CURVE()
B_SPLINE_CURVE(2,(#17754,#17755,#17756),.UNSPECIFIED.,.F.,.F.)
B_SPLINE_CURVE_WITH_KNOTS((3,3),(0.,0.0208203041102522),.UNSPECIFIED.)
CURVE()
GEOMETRIC_REPRESENTATION_ITEM()
RATIONAL_B_SPLINE_CURVE((1.,1.00198318129313,1.00207919474555))
REPRESENTATION_ITEM('')
) ;
#253 = (
BOUNDED_CURVE()
B_SPLINE_CURVE(2,(#17757,#17758,#17759),.UNSPECIFIED.,.F.,.F.)
B_SPLINE_CURVE_WITH_KNOTS((3,3),(0.0229388536477059,0.0437591577578443),
 .UNSPECIFIED.)
CURVE()
GEOMETRIC_REPRESENTATION_ITEM()
RATIONAL_B_SPLINE_CURVE((1.00207919475079,1.00198318129812,1.))
REPRESENTATION_ITEM('')
) ;
#254 = (
BOUNDED_CURVE()
B_SPLINE_CURVE(2,(#17761,#17762,#17763),.UNSPECIFIED.,.F.,.F.)
B_SPLINE_CURVE_WITH_KNOTS((3,3),(0.,0.0208203041101399),.UNSPECIFIED.)
CURVE()
GEOMETRIC_REPRESENTATION_ITEM()
RATIONAL_B_SPLINE_CURVE((1.,1.00198318129313,1.00207919474555))
REPRESENTATION_ITEM('')
) ;
#255 = (
BOUNDED_CURVE()
B_SPLINE_CURVE(2,(#17764,#17765,#17766),.UNSPECIFIED.,.F.,.F.)
B_SPLINE_CURVE_WITH_KNOTS((3,3),(0.022938853647565,0.0437591577578454),
 .UNSPECIFIED.)
CURVE()
GEOMETRIC_REPRESENTATION_ITEM()
RATIONAL_B_SPLINE_CURVE((1.00207919472218,1.00198318127084,1.))
REPRESENTATION_ITEM('')
) ;
#256 = (
BOUNDED_CURVE()
B_SPLINE_CURVE(2,(#17768,#17769,#17770),.UNSPECIFIED.,.F.,.F.)
B_SPLINE_CURVE_WITH_KNOTS((3,3),(0.,0.0208203041101981),.UNSPECIFIED.)
CURVE()
GEOMETRIC_REPRESENTATION_ITEM()
RATIONAL_B_SPLINE_CURVE((1.,1.00198318127317,1.00207919472462))
REPRESENTATION_ITEM('')
) ;
#257 = (
BOUNDED_CURVE()
B_SPLINE_CURVE(2,(#17771,#17772,#17773),.UNSPECIFIED.,.F.,.F.)
B_SPLINE_CURVE_WITH_KNOTS((3,3),(0.0229388536476133,0.0437591577578448),
 .UNSPECIFIED.)
CURVE()
GEOMETRIC_REPRESENTATION_ITEM()
RATIONAL_B_SPLINE_CURVE((1.00207919472699,1.00198318127544,1.))
REPRESENTATION_ITEM('')
) ;
#258 = (
BOUNDED_CURVE()
B_SPLINE_CURVE(2,(#17775,#17776,#17777),.UNSPECIFIED.,.F.,.F.)
B_SPLINE_CURVE_WITH_KNOTS((3,3),(0.,0.0208203041102164),.UNSPECIFIED.)
CURVE()
GEOMETRIC_REPRESENTATION_ITEM()
RATIONAL_B_SPLINE_CURVE((1.,1.00198318130011,1.00207919475286))
REPRESENTATION_ITEM('')
) ;
#259 = (
BOUNDED_CURVE()
B_SPLINE_CURVE(2,(#17778,#17779,#17780),.UNSPECIFIED.,.F.,.F.)
B_SPLINE_CURVE_WITH_KNOTS((3,3),(0.022938853647606,0.0437591577578459),
 .UNSPECIFIED.)
CURVE()
GEOMETRIC_REPRESENTATION_ITEM()
RATIONAL_B_SPLINE_CURVE((1.00207919473573,1.00198318128377,1.))
REPRESENTATION_ITEM('')
) ;
#260 = (
BOUNDED_CURVE()
B_SPLINE_CURVE(2,(#17782,#17783,#17784),.UNSPECIFIED.,.F.,.F.)
B_SPLINE_CURVE_WITH_KNOTS((3,3),(0.,0.0208203041102311),.UNSPECIFIED.)
CURVE()
GEOMETRIC_REPRESENTATION_ITEM()
RATIONAL_B_SPLINE_CURVE((1.,1.00198318129299,1.0020791947454))
REPRESENTATION_ITEM('')
) ;
#261 = (
BOUNDED_CURVE()
B_SPLINE_CURVE(2,(#17785,#17786,#17787),.UNSPECIFIED.,.F.,.F.)
B_SPLINE_CURVE_WITH_KNOTS((3,3),(0.0229388536476449,0.0437591577578444),
 .UNSPECIFIED.)
CURVE()
GEOMETRIC_REPRESENTATION_ITEM()
RATIONAL_B_SPLINE_CURVE((1.0020791947485,1.00198318129594,1.))
REPRESENTATION_ITEM('')
) ;
#262 = (
BOUNDED_CURVE()
B_SPLINE_CURVE(2,(#17789,#17790,#17791),.UNSPECIFIED.,.F.,.F.)
B_SPLINE_CURVE_WITH_KNOTS((3,3),(0.,0.0208203041101845),.UNSPECIFIED.)
CURVE()
GEOMETRIC_REPRESENTATION_ITEM()
RATIONAL_B_SPLINE_CURVE((1.,1.00198318129298,1.00207919474539))
REPRESENTATION_ITEM('')
) ;
#263 = (
BOUNDED_CURVE()
B_SPLINE_CURVE(2,(#17792,#17793,#17794),.UNSPECIFIED.,.F.,.F.)
B_SPLINE_CURVE_WITH_KNOTS((3,3),(0.0229388536476154,0.0437591577578439),
 .UNSPECIFIED.)
CURVE()
GEOMETRIC_REPRESENTATION_ITEM()
RATIONAL_B_SPLINE_CURVE((1.00207919473424,1.00198318128235,1.))
REPRESENTATION_ITEM('')
) ;
#264 = (
BOUNDED_CURVE()
B_SPLINE_CURVE(2,(#17796,#17797,#17798),.UNSPECIFIED.,.F.,.F.)
B_SPLINE_CURVE_WITH_KNOTS((3,3),(0.,0.0208203041102815),.UNSPECIFIED.)
CURVE()
GEOMETRIC_REPRESENTATION_ITEM()
RATIONAL_B_SPLINE_CURVE((1.,1.00198318127347,1.00207919472493))
REPRESENTATION_ITEM('')
) ;
#265 = (
BOUNDED_CURVE()
B_SPLINE_CURVE(2,(#17799,#17800,#17801),.UNSPECIFIED.,.F.,.F.)
B_SPLINE_CURVE_WITH_KNOTS((3,3),(0.0229388536476481,0.0437591577578452),
 .UNSPECIFIED.)
CURVE()
GEOMETRIC_REPRESENTATION_ITEM()
RATIONAL_B_SPLINE_CURVE((1.00207919474569,1.00198318129326,1.))
REPRESENTATION_ITEM('')
) ;
#266 = (
BOUNDED_CURVE()
B_SPLINE_CURVE(2,(#17803,#17804,#17805),.UNSPECIFIED.,.F.,.F.)
B_SPLINE_CURVE_WITH_KNOTS((3,3),(0.,0.0208203041101622),.UNSPECIFIED.)
CURVE()
GEOMETRIC_REPRESENTATION_ITEM()
RATIONAL_B_SPLINE_CURVE((1.,1.00198318130135,1.00207919475417))
REPRESENTATION_ITEM('')
) ;
#267 = (
BOUNDED_CURVE()
B_SPLINE_CURVE(2,(#17806,#17807,#17808),.UNSPECIFIED.,.F.,.F.)
B_SPLINE_CURVE_WITH_KNOTS((3,3),(0.0229388536475943,0.0437591577578443),
 .UNSPECIFIED.)
CURVE()
GEOMETRIC_REPRESENTATION_ITEM()
RATIONAL_B_SPLINE_CURVE((1.00207919473131,1.00198318127955,1.))
REPRESENTATION_ITEM('')
) ;
#268 = (
BOUNDED_CURVE()
B_SPLINE_CURVE(2,(#17810,#17811,#17812),.UNSPECIFIED.,.F.,.F.)
B_SPLINE_CURVE_WITH_KNOTS((3,3),(0.,0.0208203041102868),.UNSPECIFIED.)
CURVE()
GEOMETRIC_REPRESENTATION_ITEM()
RATIONAL_B_SPLINE_CURVE((1.,1.00198318127515,1.00207919472669))
REPRESENTATION_ITEM('')
) ;
#269 = (
BOUNDED_CURVE()
B_SPLINE_CURVE(2,(#17813,#17814,#17815),.UNSPECIFIED.,.F.,.F.)
B_SPLINE_CURVE_WITH_KNOTS((3,3),(0.0229388536476239,0.0437591577578459),
 .UNSPECIFIED.)
CURVE()
GEOMETRIC_REPRESENTATION_ITEM()
RATIONAL_B_SPLINE_CURVE((1.00207919474537,1.00198318129297,1.))
REPRESENTATION_ITEM('')
) ;
#270 = (
BOUNDED_CURVE()
B_SPLINE_CURVE(2,(#17817,#17818,#17819),.UNSPECIFIED.,.F.,.F.)
B_SPLINE_CURVE_WITH_KNOTS((3,3),(0.,0.0208203041102119),.UNSPECIFIED.)
CURVE()
GEOMETRIC_REPRESENTATION_ITEM()
RATIONAL_B_SPLINE_CURVE((1.,1.00198318128545,1.00207919473749))
REPRESENTATION_ITEM('')
) ;
#271 = (
BOUNDED_CURVE()
B_SPLINE_CURVE(2,(#17820,#17821,#17822),.UNSPECIFIED.,.F.,.F.)
B_SPLINE_CURVE_WITH_KNOTS((3,3),(0.022938853647645,0.0437591577578424),
 .UNSPECIFIED.)
CURVE()
GEOMETRIC_REPRESENTATION_ITEM()
RATIONAL_B_SPLINE_CURVE((1.00207919473173,1.00198318127995,1.))
REPRESENTATION_ITEM('')
) ;
#272 = (
BOUNDED_CURVE()
B_SPLINE_CURVE(2,(#17824,#17825,#17826),.UNSPECIFIED.,.F.,.F.)
B_SPLINE_CURVE_WITH_KNOTS((3,3),(0.,0.0208203041101933),.UNSPECIFIED.)
CURVE()
GEOMETRIC_REPRESENTATION_ITEM()
RATIONAL_B_SPLINE_CURVE((1.,1.00198318129507,1.00207919474759))
REPRESENTATION_ITEM('')
) ;
#273 = (
BOUNDED_CURVE()
B_SPLINE_CURVE(2,(#17827,#17828,#17829),.UNSPECIFIED.,.F.,.F.)
B_SPLINE_CURVE_WITH_KNOTS((3,3),(0.0229388536476438,0.0437591577578434),
 .UNSPECIFIED.)
CURVE()
GEOMETRIC_REPRESENTATION_ITEM()
RATIONAL_B_SPLINE_CURVE((1.00207919475882,1.00198318130579,1.))
REPRESENTATION_ITEM('')
) ;
#274 = (
BOUNDED_CURVE()
B_SPLINE_CURVE(2,(#17831,#17832,#17833),.UNSPECIFIED.,.F.,.F.)
B_SPLINE_CURVE_WITH_KNOTS((3,3),(0.,0.020820304110188),.UNSPECIFIED.)
CURVE()
GEOMETRIC_REPRESENTATION_ITEM()
RATIONAL_B_SPLINE_CURVE((1.,1.0019831812866,1.0020791947387))
REPRESENTATION_ITEM('')
) ;
#275 = (
BOUNDED_CURVE()
B_SPLINE_CURVE(2,(#17834,#17835,#17836),.UNSPECIFIED.,.F.,.F.)
B_SPLINE_CURVE_WITH_KNOTS((3,3),(0.0229388536475715,0.0437591577578452),
 .UNSPECIFIED.)
CURVE()
GEOMETRIC_REPRESENTATION_ITEM()
RATIONAL_B_SPLINE_CURVE((1.00207919474451,1.00198318129215,1.))
REPRESENTATION_ITEM('')
) ;
#276 = (
BOUNDED_CURVE()
B_SPLINE_CURVE(2,(#17838,#17839,#17840),.UNSPECIFIED.,.F.,.F.)
B_SPLINE_CURVE_WITH_KNOTS((3,3),(0.,0.0208203041102257),.UNSPECIFIED.)
CURVE()
GEOMETRIC_REPRESENTATION_ITEM()
RATIONAL_B_SPLINE_CURVE((1.,1.00198318129643,1.00207919474901))
REPRESENTATION_ITEM('')
) ;
#277 = (
BOUNDED_CURVE()
B_SPLINE_CURVE(2,(#17841,#17842,#17843),.UNSPECIFIED.,.F.,.F.)
B_SPLINE_CURVE_WITH_KNOTS((3,3),(0.0229388536476128,0.0437591577578448),
 .UNSPECIFIED.)
CURVE()
GEOMETRIC_REPRESENTATION_ITEM()
RATIONAL_B_SPLINE_CURVE((1.00207919474488,1.0019831812925,1.))
REPRESENTATION_ITEM('')
) ;
#278 = (
BOUNDED_CURVE()
B_SPLINE_CURVE(2,(#17845,#17846,#17847),.UNSPECIFIED.,.F.,.F.)
B_SPLINE_CURVE_WITH_KNOTS((3,3),(0.,0.0208203041102548),.UNSPECIFIED.)
CURVE()
GEOMETRIC_REPRESENTATION_ITEM()
RATIONAL_B_SPLINE_CURVE((1.,1.00198318128365,1.0020791947356))
REPRESENTATION_ITEM('')
) ;
#279 = (
BOUNDED_CURVE()
B_SPLINE_CURVE(2,(#17848,#17849,#17850),.UNSPECIFIED.,.F.,.F.)
B_SPLINE_CURVE_WITH_KNOTS((3,3),(0.0229388536476842,0.0437591577578424),
 .UNSPECIFIED.)
CURVE()
GEOMETRIC_REPRESENTATION_ITEM()
RATIONAL_B_SPLINE_CURVE((1.00207919473831,1.00198318128623,1.))
REPRESENTATION_ITEM('')
) ;
#280 = (
BOUNDED_CURVE()
B_SPLINE_CURVE(2,(#17852,#17853,#17854),.UNSPECIFIED.,.F.,.F.)
B_SPLINE_CURVE_WITH_KNOTS((3,3),(0.,0.0208203041101929),.UNSPECIFIED.)
CURVE()
GEOMETRIC_REPRESENTATION_ITEM()
RATIONAL_B_SPLINE_CURVE((1.,1.00198318129994,1.00207919475269))
REPRESENTATION_ITEM('')
) ;
#281 = (
BOUNDED_CURVE()
B_SPLINE_CURVE(2,(#17855,#17856,#17857),.UNSPECIFIED.,.F.,.F.)
B_SPLINE_CURVE_WITH_KNOTS((3,3),(0.0229388536476416,0.0437591577578453),
 .UNSPECIFIED.)
CURVE()
GEOMETRIC_REPRESENTATION_ITEM()
RATIONAL_B_SPLINE_CURVE((1.0020791947507,1.00198318129804,1.))
REPRESENTATION_ITEM('')
) ;
#282 = (
BOUNDED_CURVE()
B_SPLINE_CURVE(2,(#17859,#17860,#17861),.UNSPECIFIED.,.F.,.F.)
B_SPLINE_CURVE_WITH_KNOTS((3,3),(0.,0.0208203041102008),.UNSPECIFIED.)
CURVE()
GEOMETRIC_REPRESENTATION_ITEM()
RATIONAL_B_SPLINE_CURVE((1.,1.00198318128547,1.00207919473751))
REPRESENTATION_ITEM('')
) ;
#283 = (
BOUNDED_CURVE()
B_SPLINE_CURVE(2,(#17862,#17863,#17864),.UNSPECIFIED.,.F.,.F.)
B_SPLINE_CURVE_WITH_KNOTS((3,3),(0.0229388536475931,0.0437591577578445),
 .UNSPECIFIED.)
CURVE()
GEOMETRIC_REPRESENTATION_ITEM()
RATIONAL_B_SPLINE_CURVE((1.00207919474108,1.00198318128887,1.))
REPRESENTATION_ITEM('')
) ;
#284 = (
BOUNDED_CURVE()
B_SPLINE_CURVE(2,(#17866,#17867,#17868),.UNSPECIFIED.,.F.,.F.)
B_SPLINE_CURVE_WITH_KNOTS((3,3),(0.,0.0208203041102136),.UNSPECIFIED.)
CURVE()
GEOMETRIC_REPRESENTATION_ITEM()
RATIONAL_B_SPLINE_CURVE((1.,1.00198318127179,1.00207919472318))
REPRESENTATION_ITEM('')
) ;
#285 = (
BOUNDED_CURVE()
B_SPLINE_CURVE(2,(#17869,#17870,#17871),.UNSPECIFIED.,.F.,.F.)
B_SPLINE_CURVE_WITH_KNOTS((3,3),(0.0229388536475417,0.0437591577578453),
 .UNSPECIFIED.)
CURVE()
GEOMETRIC_REPRESENTATION_ITEM()
RATIONAL_B_SPLINE_CURVE((1.00207919475326,1.0019831813005,1.))
REPRESENTATION_ITEM('')
) ;
#286 = (
BOUNDED_CURVE()
B_SPLINE_CURVE(2,(#17873,#17874,#17875),.UNSPECIFIED.,.F.,.F.)
B_SPLINE_CURVE_WITH_KNOTS((3,3),(0.,0.0208203041102395),.UNSPECIFIED.)
CURVE()
GEOMETRIC_REPRESENTATION_ITEM()
RATIONAL_B_SPLINE_CURVE((1.,1.00198318130368,1.0020791947566))
REPRESENTATION_ITEM('')
) ;
#287 = (
BOUNDED_CURVE()
B_SPLINE_CURVE(2,(#17876,#17877,#17878),.UNSPECIFIED.,.F.,.F.)
B_SPLINE_CURVE_WITH_KNOTS((3,3),(0.0229388536476164,0.0437591577578449),
 .UNSPECIFIED.)
CURVE()
GEOMETRIC_REPRESENTATION_ITEM()
RATIONAL_B_SPLINE_CURVE((1.00207919474665,1.00198318129418,1.))
REPRESENTATION_ITEM('')
) ;
#288 = (
BOUNDED_CURVE()
B_SPLINE_CURVE(2,(#17880,#17881,#17882),.UNSPECIFIED.,.F.,.F.)
B_SPLINE_CURVE_WITH_KNOTS((3,3),(0.,0.0208203041102497),.UNSPECIFIED.)
CURVE()
GEOMETRIC_REPRESENTATION_ITEM()
RATIONAL_B_SPLINE_CURVE((1.,1.00198318126206,1.00207919471297))
REPRESENTATION_ITEM('')
) ;
#289 = (
BOUNDED_CURVE()
B_SPLINE_CURVE(2,(#17883,#17884,#17885),.UNSPECIFIED.,.F.,.F.)
B_SPLINE_CURVE_WITH_KNOTS((3,3),(0.0229388536475813,0.0437591577578465),
 .UNSPECIFIED.)
CURVE()
GEOMETRIC_REPRESENTATION_ITEM()
RATIONAL_B_SPLINE_CURVE((1.00207919474568,1.00198318129326,1.))
REPRESENTATION_ITEM('')
) ;
#290 = (
BOUNDED_CURVE()
B_SPLINE_CURVE(2,(#17887,#17888,#17889),.UNSPECIFIED.,.F.,.F.)
B_SPLINE_CURVE_WITH_KNOTS((3,3),(0.,0.0208203041102125),.UNSPECIFIED.)
CURVE()
GEOMETRIC_REPRESENTATION_ITEM()
RATIONAL_B_SPLINE_CURVE((1.,1.00198318129832,1.00207919475098))
REPRESENTATION_ITEM('')
) ;
#291 = (
BOUNDED_CURVE()
B_SPLINE_CURVE(2,(#17890,#17891,#17892),.UNSPECIFIED.,.F.,.F.)
B_SPLINE_CURVE_WITH_KNOTS((3,3),(0.0229388536475884,0.043759157757846),
 .UNSPECIFIED.)
CURVE()
GEOMETRIC_REPRESENTATION_ITEM()
RATIONAL_B_SPLINE_CURVE((1.00207919473695,1.00198318128494,1.))
REPRESENTATION_ITEM('')
) ;
#292 = (
BOUNDED_CURVE()
B_SPLINE_CURVE(2,(#17894,#17895,#17896),.UNSPECIFIED.,.F.,.F.)
B_SPLINE_CURVE_WITH_KNOTS((3,3),(0.,0.0208203041102161),.UNSPECIFIED.)
CURVE()
GEOMETRIC_REPRESENTATION_ITEM()
RATIONAL_B_SPLINE_CURVE((1.,1.00198318130551,1.00207919475853))
REPRESENTATION_ITEM('')
) ;
#293 = (
BOUNDED_CURVE()
B_SPLINE_CURVE(2,(#17897,#17898,#17899),.UNSPECIFIED.,.F.,.F.)
B_SPLINE_CURVE_WITH_KNOTS((3,3),(0.0229388536476204,0.0437591577578463),
 .UNSPECIFIED.)
CURVE()
GEOMETRIC_REPRESENTATION_ITEM()
RATIONAL_B_SPLINE_CURVE((1.00207919473782,1.00198318128577,1.))
REPRESENTATION_ITEM('')
) ;
#294 = (
BOUNDED_CURVE()
B_SPLINE_CURVE(2,(#17901,#17902,#17903),.UNSPECIFIED.,.F.,.F.)
B_SPLINE_CURVE_WITH_KNOTS((3,3),(0.,0.0208203041102228),.UNSPECIFIED.)
CURVE()
GEOMETRIC_REPRESENTATION_ITEM()
RATIONAL_B_SPLINE_CURVE((1.,1.00198318128961,1.00207919474186))
REPRESENTATION_ITEM('')
) ;
#295 = (
BOUNDED_CURVE()
B_SPLINE_CURVE(2,(#17904,#17905,#17906),.UNSPECIFIED.,.F.,.F.)
B_SPLINE_CURVE_WITH_KNOTS((3,3),(0.0229388536476005,0.0437591577578455),
 .UNSPECIFIED.)
CURVE()
GEOMETRIC_REPRESENTATION_ITEM()
RATIONAL_B_SPLINE_CURVE((1.00207919472128,1.00198318126998,1.))
REPRESENTATION_ITEM('')
) ;
#296 = (
BOUNDED_CURVE()
B_SPLINE_CURVE(2,(#17908,#17909,#17910),.UNSPECIFIED.,.F.,.F.)
B_SPLINE_CURVE_WITH_KNOTS((3,3),(0.,0.0208203041102323),.UNSPECIFIED.)
CURVE()
GEOMETRIC_REPRESENTATION_ITEM()
RATIONAL_B_SPLINE_CURVE((1.,1.00198318129082,1.00207919474313))
REPRESENTATION_ITEM('')
) ;
#297 = (
BOUNDED_CURVE()
B_SPLINE_CURVE(2,(#17911,#17912,#17913),.UNSPECIFIED.,.F.,.F.)
B_SPLINE_CURVE_WITH_KNOTS((3,3),(0.0229388536476069,0.0437591577578452),
 .UNSPECIFIED.)
CURVE()
GEOMETRIC_REPRESENTATION_ITEM()
RATIONAL_B_SPLINE_CURVE((1.00207919474246,1.00198318129019,1.))
REPRESENTATION_ITEM('')
) ;
#298 = (
BOUNDED_CURVE()
B_SPLINE_CURVE(2,(#17915,#17916,#17917),.UNSPECIFIED.,.F.,.F.)
B_SPLINE_CURVE_WITH_KNOTS((3,3),(0.,0.0208203041102477),.UNSPECIFIED.)
CURVE()
GEOMETRIC_REPRESENTATION_ITEM()
RATIONAL_B_SPLINE_CURVE((1.,1.00198318127836,1.00207919473006))
REPRESENTATION_ITEM('')
) ;
#299 = (
BOUNDED_CURVE()
B_SPLINE_CURVE(2,(#17918,#17919,#17920),.UNSPECIFIED.,.F.,.F.)
B_SPLINE_CURVE_WITH_KNOTS((3,3),(0.0229388536476238,0.0437591577578459),
 .UNSPECIFIED.)
CURVE()
GEOMETRIC_REPRESENTATION_ITEM()
RATIONAL_B_SPLINE_CURVE((1.0020791947311,1.00198318127935,1.))
REPRESENTATION_ITEM('')
) ;
#300 = (
BOUNDED_CURVE()
B_SPLINE_CURVE(2,(#17922,#17923,#17924),.UNSPECIFIED.,.F.,.F.)
B_SPLINE_CURVE_WITH_KNOTS((3,3),(0.,0.0208203041102102),.UNSPECIFIED.)
CURVE()
GEOMETRIC_REPRESENTATION_ITEM()
RATIONAL_B_SPLINE_CURVE((1.,1.00198318128188,1.00207919473375))
REPRESENTATION_ITEM('')
) ;
#301 = (
BOUNDED_CURVE()
B_SPLINE_CURVE(2,(#17925,#17926,#17927),.UNSPECIFIED.,.F.,.F.)
B_SPLINE_CURVE_WITH_KNOTS((3,3),(0.0229388536476158,0.0437591577578472),
 .UNSPECIFIED.)
CURVE()
GEOMETRIC_REPRESENTATION_ITEM()
RATIONAL_B_SPLINE_CURVE((1.00207919475336,1.00198318130059,1.))
REPRESENTATION_ITEM('')
) ;
#302 = (
BOUNDED_CURVE()
B_SPLINE_CURVE(2,(#17929,#17930,#17931),.UNSPECIFIED.,.F.,.F.)
B_SPLINE_CURVE_WITH_KNOTS((3,3),(0.,0.0208203041102333),.UNSPECIFIED.)
CURVE()
GEOMETRIC_REPRESENTATION_ITEM()
RATIONAL_B_SPLINE_CURVE((1.,1.00198318128675,1.00207919473886))
REPRESENTATION_ITEM('')
) ;
#303 = (
BOUNDED_CURVE()
B_SPLINE_CURVE(2,(#17932,#17933,#17934),.UNSPECIFIED.,.F.,.F.)
B_SPLINE_CURVE_WITH_KNOTS((3,3),(0.0229388536476674,0.0437591577578436),
 .UNSPECIFIED.)
CURVE()
GEOMETRIC_REPRESENTATION_ITEM()
RATIONAL_B_SPLINE_CURVE((1.00207919473716,1.00198318128513,1.))
REPRESENTATION_ITEM('')
) ;
#304 = (
BOUNDED_CURVE()
B_SPLINE_CURVE(2,(#17936,#17937,#17938),.UNSPECIFIED.,.F.,.F.)
B_SPLINE_CURVE_WITH_KNOTS((3,3),(0.,0.0208203041101914),.UNSPECIFIED.)
CURVE()
GEOMETRIC_REPRESENTATION_ITEM()
RATIONAL_B_SPLINE_CURVE((1.,1.00198318129795,1.00207919475061))
REPRESENTATION_ITEM('')
) ;
#305 = (
BOUNDED_CURVE()
B_SPLINE_CURVE(2,(#17939,#17940,#17941),.UNSPECIFIED.,.F.,.F.)
B_SPLINE_CURVE_WITH_KNOTS((3,3),(0.0229388536476256,0.0437591577578441),
 .UNSPECIFIED.)
CURVE()
GEOMETRIC_REPRESENTATION_ITEM()
RATIONAL_B_SPLINE_CURVE((1.00207919474269,1.00198318129041,1.))
REPRESENTATION_ITEM('')
) ;
#306 = (
BOUNDED_CURVE()
B_SPLINE_CURVE(2,(#17943,#17944,#17945),.UNSPECIFIED.,.F.,.F.)
B_SPLINE_CURVE_WITH_KNOTS((3,3),(0.,0.0208203041102649),.UNSPECIFIED.)
CURVE()
GEOMETRIC_REPRESENTATION_ITEM()
RATIONAL_B_SPLINE_CURVE((1.,1.00198318128372,1.00207919473568))
REPRESENTATION_ITEM('')
) ;
#307 = (
BOUNDED_CURVE()
B_SPLINE_CURVE(2,(#17946,#17947,#17948),.UNSPECIFIED.,.F.,.F.)
B_SPLINE_CURVE_WITH_KNOTS((3,3),(0.0229388536476116,0.0437591577578462),
 .UNSPECIFIED.)
CURVE()
GEOMETRIC_REPRESENTATION_ITEM()
RATIONAL_B_SPLINE_CURVE((1.00207919474123,1.00198318128901,1.))
REPRESENTATION_ITEM('')
) ;
#308 = (
BOUNDED_CURVE()
B_SPLINE_CURVE(2,(#17950,#17951,#17952),.UNSPECIFIED.,.F.,.F.)
B_SPLINE_CURVE_WITH_KNOTS((3,3),(0.,0.0208203041102467),.UNSPECIFIED.)
CURVE()
GEOMETRIC_REPRESENTATION_ITEM()
RATIONAL_B_SPLINE_CURVE((1.,1.00198318128474,1.00207919473675))
REPRESENTATION_ITEM('')
) ;
#309 = (
BOUNDED_CURVE()
B_SPLINE_CURVE(2,(#17953,#17954,#17955),.UNSPECIFIED.,.F.,.F.)
B_SPLINE_CURVE_WITH_KNOTS((3,3),(0.0229388536476399,0.0437591577578457),
 .UNSPECIFIED.)
CURVE()
GEOMETRIC_REPRESENTATION_ITEM()
RATIONAL_B_SPLINE_CURVE((1.00207919474381,1.00198318129148,1.))
REPRESENTATION_ITEM('')
) ;
#310 = (
BOUNDED_CURVE()
B_SPLINE_CURVE(2,(#17957,#17958,#17959),.UNSPECIFIED.,.F.,.F.)
B_SPLINE_CURVE_WITH_KNOTS((3,3),(0.,0.0208203041102079),.UNSPECIFIED.)
CURVE()
GEOMETRIC_REPRESENTATION_ITEM()
RATIONAL_B_SPLINE_CURVE((1.,1.00198318129612,1.00207919474868))
REPRESENTATION_ITEM('')
) ;
#311 = (
BOUNDED_CURVE()
B_SPLINE_CURVE(2,(#17960,#17961,#17962),.UNSPECIFIED.,.F.,.F.)
B_SPLINE_CURVE_WITH_KNOTS((3,3),(0.0229388536475489,0.043759157757846),
 .UNSPECIFIED.)
CURVE()
GEOMETRIC_REPRESENTATION_ITEM()
RATIONAL_B_SPLINE_CURVE((1.00207919471265,1.00198318126176,1.))
REPRESENTATION_ITEM('')
) ;
#312 = (
BOUNDED_CURVE()
B_SPLINE_CURVE(2,(#17964,#17965,#17966),.UNSPECIFIED.,.F.,.F.)
B_SPLINE_CURVE_WITH_KNOTS((3,3),(0.,0.020820304110324),.UNSPECIFIED.)
CURVE()
GEOMETRIC_REPRESENTATION_ITEM()
RATIONAL_B_SPLINE_CURVE((1.,1.00198318127347,1.00207919472492))
REPRESENTATION_ITEM('')
) ;
#313 = (
BOUNDED_CURVE()
B_SPLINE_CURVE(2,(#17967,#17968,#17969),.UNSPECIFIED.,.F.,.F.)
B_SPLINE_CURVE_WITH_KNOTS((3,3),(0.0229388536476511,0.0437591577578447),
 .UNSPECIFIED.)
CURVE()
GEOMETRIC_REPRESENTATION_ITEM()
RATIONAL_B_SPLINE_CURVE((1.00207919473721,1.00198318128518,1.))
REPRESENTATION_ITEM('')
) ;
#314 = (
BOUNDED_CURVE()
B_SPLINE_CURVE(2,(#17971,#17972,#17973),.UNSPECIFIED.,.F.,.F.)
B_SPLINE_CURVE_WITH_KNOTS((3,3),(0.,0.0208203041102687),.UNSPECIFIED.)
CURVE()
GEOMETRIC_REPRESENTATION_ITEM()
RATIONAL_B_SPLINE_CURVE((1.,1.00198318127639,1.002079194728))
REPRESENTATION_ITEM('')
) ;
#315 = (
BOUNDED_CURVE()
B_SPLINE_CURVE(2,(#17974,#17975,#17976),.UNSPECIFIED.,.F.,.F.)
B_SPLINE_CURVE_WITH_KNOTS((3,3),(0.0229388536475813,0.0437591577578468),
 .UNSPECIFIED.)
CURVE()
GEOMETRIC_REPRESENTATION_ITEM()
RATIONAL_B_SPLINE_CURVE((1.00207919473967,1.00198318128753,1.))
REPRESENTATION_ITEM('')
) ;
#316 = (
BOUNDED_CURVE()
B_SPLINE_CURVE(2,(#17978,#17979,#17980),.UNSPECIFIED.,.F.,.F.)
B_SPLINE_CURVE_WITH_KNOTS((3,3),(0.,0.020820304110235),.UNSPECIFIED.)
CURVE()
GEOMETRIC_REPRESENTATION_ITEM()
RATIONAL_B_SPLINE_CURVE((1.,1.00198318129245,1.00207919474483))
REPRESENTATION_ITEM('')
) ;
#317 = (
BOUNDED_CURVE()
B_SPLINE_CURVE(2,(#17981,#17982,#17983),.UNSPECIFIED.,.F.,.F.)
B_SPLINE_CURVE_WITH_KNOTS((3,3),(0.0229388536476187,0.0437591577578467),
 .UNSPECIFIED.)
CURVE()
GEOMETRIC_REPRESENTATION_ITEM()
RATIONAL_B_SPLINE_CURVE((1.00207919475315,1.00198318130038,1.))
REPRESENTATION_ITEM('')
) ;
#318 = (
BOUNDED_CURVE()
B_SPLINE_CURVE(2,(#17984,#17985,#17986),.UNSPECIFIED.,.F.,.F.)
B_SPLINE_CURVE_WITH_KNOTS((3,3),(0.,0.0208203041103129),.UNSPECIFIED.)
CURVE()
GEOMETRIC_REPRESENTATION_ITEM()
RATIONAL_B_SPLINE_CURVE((1.,1.00198318126409,1.00207919471509))
REPRESENTATION_ITEM('')
) ;
#319 = (
BOUNDED_CURVE()
B_SPLINE_CURVE(2,(#18234,#18235,#18236),.UNSPECIFIED.,.F.,.F.)
B_SPLINE_CURVE_WITH_KNOTS((3,3),(0.,0.0136874154102615),.UNSPECIFIED.)
CURVE()
GEOMETRIC_REPRESENTATION_ITEM()
RATIONAL_B_SPLINE_CURVE((1.,1.0066910623624,1.00897713804962))
REPRESENTATION_ITEM('')
) ;
#320 = (
BOUNDED_CURVE()
B_SPLINE_CURVE(2,(#18240,#18241,#18242),.UNSPECIFIED.,.F.,.F.)
B_SPLINE_CURVE_WITH_KNOTS((3,3),(0.0278942541126724,0.0415816695229389),
 .UNSPECIFIED.)
CURVE()
GEOMETRIC_REPRESENTATION_ITEM()
RATIONAL_B_SPLINE_CURVE((1.00897713804904,1.00669106236197,1.))
REPRESENTATION_ITEM('')
) ;
#321 = (
BOUNDED_CURVE()
B_SPLINE_CURVE(2,(#18244,#18245,#18246),.UNSPECIFIED.,.F.,.F.)
B_SPLINE_CURVE_WITH_KNOTS((3,3),(0.,0.0136874154102685),.UNSPECIFIED.)
CURVE()
GEOMETRIC_REPRESENTATION_ITEM()
RATIONAL_B_SPLINE_CURVE((1.,1.00669106236162,1.00897713804858))
REPRESENTATION_ITEM('')
) ;
#322 = (
BOUNDED_CURVE()
B_SPLINE_CURVE(2,(#18250,#18251,#18252),.UNSPECIFIED.,.F.,.F.)
B_SPLINE_CURVE_WITH_KNOTS((3,3),(0.0278942541126688,0.0415816695229383),
 .UNSPECIFIED.)
CURVE()
GEOMETRIC_REPRESENTATION_ITEM()
RATIONAL_B_SPLINE_CURVE((1.00897713804858,1.00669106236162,1.))
REPRESENTATION_ITEM('')
) ;
#323 = (
BOUNDED_CURVE()
B_SPLINE_CURVE(2,(#18254,#18255,#18256),.UNSPECIFIED.,.F.,.F.)
B_SPLINE_CURVE_WITH_KNOTS((3,3),(0.,0.0136874154102617),.UNSPECIFIED.)
CURVE()
GEOMETRIC_REPRESENTATION_ITEM()
RATIONAL_B_SPLINE_CURVE((1.,1.0066910623619,1.00897713804895))
REPRESENTATION_ITEM('')
) ;
#324 = (
BOUNDED_CURVE()
B_SPLINE_CURVE(2,(#18260,#18261,#18262),.UNSPECIFIED.,.F.,.F.)
B_SPLINE_CURVE_WITH_KNOTS((3,3),(0.0278942541126742,0.0415816695229357),
 .UNSPECIFIED.)
CURVE()
GEOMETRIC_REPRESENTATION_ITEM()
RATIONAL_B_SPLINE_CURVE((1.0089771380487,1.00669106236171,1.))
REPRESENTATION_ITEM('')
) ;
#325 = (
BOUNDED_CURVE()
B_SPLINE_CURVE(2,(#18264,#18265,#18266),.UNSPECIFIED.,.F.,.F.)
B_SPLINE_CURVE_WITH_KNOTS((3,3),(0.,0.0136874154102619),.UNSPECIFIED.)
CURVE()
GEOMETRIC_REPRESENTATION_ITEM()
RATIONAL_B_SPLINE_CURVE((1.,1.00669106236241,1.00897713804963))
REPRESENTATION_ITEM('')
) ;
#326 = (
BOUNDED_CURVE()
B_SPLINE_CURVE(2,(#18270,#18271,#18272),.UNSPECIFIED.,.F.,.F.)
B_SPLINE_CURVE_WITH_KNOTS((3,3),(0.0278942541126735,0.0415816695229364),
 .UNSPECIFIED.)
CURVE()
GEOMETRIC_REPRESENTATION_ITEM()
RATIONAL_B_SPLINE_CURVE((1.00897713804995,1.00669106236265,1.))
REPRESENTATION_ITEM('')
) ;
#327 = (
BOUNDED_CURVE()
B_SPLINE_CURVE(2,(#18274,#18275,#18276),.UNSPECIFIED.,.F.,.F.)
B_SPLINE_CURVE_WITH_KNOTS((3,3),(0.,0.0136874154102649),.UNSPECIFIED.)
CURVE()
GEOMETRIC_REPRESENTATION_ITEM()
RATIONAL_B_SPLINE_CURVE((1.,1.00669106236169,1.00897713804866))
REPRESENTATION_ITEM('')
) ;
#328 = (
BOUNDED_CURVE()
B_SPLINE_CURVE(2,(#18280,#18281,#18282),.UNSPECIFIED.,.F.,.F.)
B_SPLINE_CURVE_WITH_KNOTS((3,3),(0.0278942541126746,0.0415816695229368),
 .UNSPECIFIED.)
CURVE()
GEOMETRIC_REPRESENTATION_ITEM()
RATIONAL_B_SPLINE_CURVE((1.00897713804866,1.00669106236168,1.))
REPRESENTATION_ITEM('')
) ;
#329 = (
BOUNDED_CURVE()
B_SPLINE_CURVE(2,(#18284,#18285,#18286),.UNSPECIFIED.,.F.,.F.)
B_SPLINE_CURVE_WITH_KNOTS((3,3),(0.,0.0136874154102616),.UNSPECIFIED.)
CURVE()
GEOMETRIC_REPRESENTATION_ITEM()
RATIONAL_B_SPLINE_CURVE((1.,1.00669106236177,1.00897713804877))
REPRESENTATION_ITEM('')
) ;
#330 = (
BOUNDED_CURVE()
B_SPLINE_CURVE(2,(#18289,#18290,#18291),.UNSPECIFIED.,.F.,.F.)
B_SPLINE_CURVE_WITH_KNOTS((3,3),(0.0278942541126769,0.0415816695229329),
 .UNSPECIFIED.)
CURVE()
GEOMETRIC_REPRESENTATION_ITEM()
RATIONAL_B_SPLINE_CURVE((1.00897713804978,1.00669106236252,1.))
REPRESENTATION_ITEM('')
) ;
#331 = TOROIDAL_SURFACE('',#9944,5.50000000000001,0.5) ;
#332 = TOROIDAL_SURFACE('',#9950,5.50000000000001,0.5) ;
#333 = TOROIDAL_SURFACE('',#9956,5.50000000000001,0.5) ;
#334 = TOROIDAL_SURFACE('',#9962,5.50000000000001,0.5) ;
#335 = TOROIDAL_SURFACE('',#10190,10.,2.85) ;
#336 = TOROIDAL_SURFACE('',#10197,10.,2.85) ;
#337 = TOROIDAL_SURFACE('',#10309,1.06675,0.1) ;
#338 = TOROIDAL_SURFACE('',#10504,1.69999999999999,0.2) ;
#339 = SHAPE_REPRESENTATION_RELATIONSHIP('SRR','None',#18857,#356) ;
#340 = SHAPE_REPRESENTATION_RELATIONSHIP('SRR','None',#18858,#357) ;
#341 = SHAPE_REPRESENTATION_RELATIONSHIP('SRR','None',#18859,#358) ;
#342 = SHAPE_REPRESENTATION_RELATIONSHIP('SRR','None',#18860,#359) ;
#343 = SHAPE_REPRESENTATION_RELATIONSHIP('SRR','None',#18861,#360) ;
#344 = SHAPE_REPRESENTATION_RELATIONSHIP('SRR','None',#18862,#361) ;
#345 = SHAPE_REPRESENTATION_RELATIONSHIP('SRR','None',#18863,#362) ;
#346 = SHAPE_REPRESENTATION_RELATIONSHIP('SRR','None',#18864,#363) ;
#347 = SHAPE_REPRESENTATION_RELATIONSHIP('SRR','None',#18865,#364) ;
#348 = SHAPE_REPRESENTATION_RELATIONSHIP('SRR','None',#18866,#365) ;
#349 = SHAPE_REPRESENTATION_RELATIONSHIP('SRR','None',#18867,#366) ;
#350 = SHAPE_REPRESENTATION_RELATIONSHIP('SRR','None',#18868,#367) ;
#351 = SHAPE_REPRESENTATION_RELATIONSHIP('SRR','None',#18869,#368) ;
#352 = SHAPE_REPRESENTATION_RELATIONSHIP('SRR','None',#18870,#369) ;
#353 = SHAPE_REPRESENTATION_RELATIONSHIP('SRR','None',#18871,#370) ;
#354 = SHAPE_REPRESENTATION_RELATIONSHIP('SRR','None',#18872,#371) ;
#355 = SHAPE_REPRESENTATION_RELATIONSHIP('SRR','None',#18873,#372) ;
#356 = ADVANCED_BREP_SHAPE_REPRESENTATION('',(#390),#18740) ;
#357 = ADVANCED_BREP_SHAPE_REPRESENTATION('',(#391),#18741) ;
#358 = ADVANCED_BREP_SHAPE_REPRESENTATION('',(#392),#18742) ;
#359 = ADVANCED_BREP_SHAPE_REPRESENTATION('',(#393),#18743) ;
#360 = ADVANCED_BREP_SHAPE_REPRESENTATION('',(#394),#18744) ;
#361 = ADVANCED_BREP_SHAPE_REPRESENTATION('',(#395),#18745) ;
#362 = ADVANCED_BREP_SHAPE_REPRESENTATION('',(#396),#18746) ;
#363 = ADVANCED_BREP_SHAPE_REPRESENTATION('',(#397),#18747) ;
#364 = ADVANCED_BREP_SHAPE_REPRESENTATION('',(#398),#18748) ;
#365 = ADVANCED_BREP_SHAPE_REPRESENTATION('',(#399),#18749) ;
#366 = ADVANCED_BREP_SHAPE_REPRESENTATION('',(#400),#18750) ;
#367 = ADVANCED_BREP_SHAPE_REPRESENTATION('',(#401),#18751) ;
#368 = ADVANCED_BREP_SHAPE_REPRESENTATION('',(#402),#18752) ;
#369 = ADVANCED_BREP_SHAPE_REPRESENTATION('',(#403),#18753) ;
#370 = ADVANCED_BREP_SHAPE_REPRESENTATION('',(#404),#18754) ;
#371 = ADVANCED_BREP_SHAPE_REPRESENTATION('',(#405),#18755) ;
#372 = ADVANCED_BREP_SHAPE_REPRESENTATION('',(#406),#18756) ;
#373 = STYLED_ITEM('',(#18951),#390) ;
#374 = STYLED_ITEM('',(#18952),#391) ;
#375 = STYLED_ITEM('',(#18953),#392) ;
#376 = STYLED_ITEM('',(#18954),#393) ;
#377 = STYLED_ITEM('',(#18955),#394) ;
#378 = STYLED_ITEM('',(#18956),#395) ;
#379 = STYLED_ITEM('',(#18957),#396) ;
#380 = STYLED_ITEM('',(#18958),#397) ;
#381 = STYLED_ITEM('',(#18959),#398) ;
#382 = STYLED_ITEM('',(#18960),#399) ;
#383 = STYLED_ITEM('',(#18961),#400) ;
#384 = STYLED_ITEM('',(#18962),#401) ;
#385 = STYLED_ITEM('',(#18963),#402) ;
#386 = STYLED_ITEM('',(#18964),#403) ;
#387 = STYLED_ITEM('',(#18965),#404) ;
#388 = STYLED_ITEM('',(#18966),#405) ;
#389 = STYLED_ITEM('',(#18967),#406) ;
#390 = MANIFOLD_SOLID_BREP('Lift Table Base Frame Weldment',#9542) ;
#391 = MANIFOLD_SOLID_BREP('Lift Table Top 14 ga with Pivot Lugs',#9543) ;
#392 = MANIFOLD_SOLID_BREP('Outer Scissor Arm Frame',#9544) ;
#393 = MANIFOLD_SOLID_BREP('Inner Scissor Arm Frame',#9545) ;
#394 = MANIFOLD_SOLID_BREP('Hydraulic Cylinder Body',#9546) ;
#395 = MANIFOLD_SOLID_BREP('Hydraulic Piston Rod with Eye',#9547) ;
#396 = MANIFOLD_SOLID_BREP('Hydraulic Foot Pump Body',#9548) ;
#397 = MANIFOLD_SOLID_BREP('Foot Pump Pedal',#9549) ;
#398 = MANIFOLD_SOLID_BREP('Push Handle (chrome tube)',#9550) ;
#399 = MANIFOLD_SOLID_BREP('Lowering Release Lever',#9551) ;
#400 = MANIFOLD_SOLID_BREP('Pivot Pin D4 x 11.4 with E-Clip Groove',#9552) ;
#401 = MANIFOLD_SOLID_BREP('DIN 6799 - 3.2 Retaining Washer (E-Clip)',#9553) ;
#402 = MANIFOLD_SOLID_BREP('Track Roller D8 with Stud',#9554) ;
#403 = MANIFOLD_SOLID_BREP('ISO 4762 - M2 x 6 - 12.9',#9555) ;
#404 = MANIFOLD_SOLID_BREP('Swivel Caster Yoke 4 in',#9556) ;
#405 = MANIFOLD_SOLID_BREP('Rigid Caster Yoke 4 in',#9557) ;
#406 = MANIFOLD_SOLID_BREP('Caster Wheel 4 in Rubber',#9558) ;
#407 = B_SPLINE_CURVE_WITH_KNOTS('',3,(#13518,#13519,#13520,#13521,#13522,
#13523,#13524,#13525,#13526,#13527,#13528,#13529,#13530,#13531,#13532,#13533,
#13534,#13535,#13536,#13537,#13538,#13539,#13540,#13541,#13542,#13543,#13544,
#13545,#13546,#13547,#13548,#13549,#13550,#13551,#13552),.UNSPECIFIED.,
 .F.,.F.,(4,2,2,2,2,2,2,2,3,2,2,2,2,2,2,2,4),(0.344577820460866,0.365980688401704,
0.406814525836436,0.448673337816236,0.490532149796036,0.530173091565364,
0.569814033334692,0.610053867634319,0.650293701933945,0.690533536233571,
0.730773370533197,0.770414312302526,0.810055254071854,0.851914066051654,
0.893772878031454,0.934606715466186,0.956009583407023),.UNSPECIFIED.) ;
#408 = B_SPLINE_CURVE_WITH_KNOTS('',3,(#13564,#13565,#13566,#13567,#13568,
#13569,#13570,#13571,#13572,#13573,#13574,#13575,#13576,#13577,#13578,#13579,
#13580,#13581,#13582,#13583,#13584,#13585,#13586,#13587,#13588,#13589,#13590,
#13591,#13592,#13593,#13594,#13595,#13596,#13597,#13598),.UNSPECIFIED.,
 .F.,.F.,(4,2,2,2,2,2,2,2,3,2,2,2,2,2,2,2,4),(0.344577820460867,0.365980688401704,
0.406814525836436,0.448673337816236,0.490532149796036,0.530173091565364,
0.569814033334692,0.610053867634319,0.650293701933945,0.690533536233571,
0.730773370533197,0.770414312302526,0.810055254071854,0.851914066051654,
0.893772878031454,0.934606715466186,0.956009583407027),.UNSPECIFIED.) ;
#409 = B_SPLINE_CURVE_WITH_KNOTS('',3,(#13629,#13630,#13631,#13632,#13633,
#13634,#13635),.UNSPECIFIED.,.F.,.F.,(4,3,4),(-0.0190556203788655,0.,0.0190556203788683),
 .UNSPECIFIED.) ;
#410 = B_SPLINE_CURVE_WITH_KNOTS('',3,(#13646,#13647,#13648,#13649,#13650,
#13651,#13652),.UNSPECIFIED.,.F.,.F.,(4,3,4),(-0.019055620378868,0.,0.0190556203788661),
 .UNSPECIFIED.) ;
#411 = B_SPLINE_CURVE_WITH_KNOTS('',3,(#13665,#13666,#13667,#13668,#13669,
#13670,#13671,#13672,#13673,#13674),.UNSPECIFIED.,.F.,.F.,(4,2,2,2,4),(0.,
0.0435910279952308,0.0871820559904617,0.130762210503654,0.174342365016846),
 .UNSPECIFIED.) ;
#412 = B_SPLINE_CURVE_WITH_KNOTS('',3,(#13675,#13676,#13677,#13678,#13679,
#13680,#13681,#13682,#13683,#13684,#13685,#13686,#13687,#13688,#13689,#13690,
#13691,#13692,#13693,#13694,#13695,#13696,#13697,#13698,#13699,#13700),
 .UNSPECIFIED.,.F.,.F.,(4,2,2,2,2,2,2,2,2,2,2,2,4),(0.174342365016846,0.217922519530038,
0.261502674043231,0.305093702038462,0.348684730033692,0.392275758028923,
0.435866786024154,0.479446940537346,0.523027095050539,0.566607249563731,
0.610187404076923,0.653778432072154,0.697369460067385),.UNSPECIFIED.) ;
#413 = B_SPLINE_CURVE_WITH_KNOTS('',3,(#13704,#13705,#13706,#13707,#13708,
#13709,#13710,#13711,#13712,#13713),.UNSPECIFIED.,.F.,.F.,(4,2,2,2,4),(0.,
0.0438474980267263,0.0876949960534527,0.131502815085544,0.175310634117636),
 .UNSPECIFIED.) ;
#414 = B_SPLINE_CURVE_WITH_KNOTS('',3,(#13714,#13715,#13716,#13717,#13718,
#13719,#13720,#13721,#13722,#13723,#13724,#13725,#13726,#13727,#13728,#13729,
#13730,#13731,#13732,#13733,#13734,#13735,#13736,#13737,#13738,#13739),
 .UNSPECIFIED.,.F.,.F.,(4,2,2,2,2,2,2,2,2,2,2,2,4),(0.175310634117636,0.219118453149728,
0.26292627218182,0.306773770208546,0.350621268235272,0.394468766261999,
0.438316264288725,0.482124083320817,0.525931902352908,0.569739721385,0.613547540417092,
0.657395038443818,0.701242536470545),.UNSPECIFIED.) ;
#415 = B_SPLINE_CURVE_WITH_KNOTS('',3,(#13750,#13751,#13752,#13753,#13754,
#13755,#13756,#13757,#13758,#13759),.UNSPECIFIED.,.F.,.F.,(4,2,2,2,4),(0.,
0.0435910279952308,0.0871820559904617,0.130762210503654,0.174342365016846),
 .UNSPECIFIED.) ;
#416 = B_SPLINE_CURVE_WITH_KNOTS('',3,(#13760,#13761,#13762,#13763,#13764,
#13765,#13766,#13767,#13768,#13769,#13770,#13771,#13772,#13773,#13774,#13775,
#13776,#13777,#13778,#13779,#13780,#13781,#13782,#13783,#13784,#13785),
 .UNSPECIFIED.,.F.,.F.,(4,2,2,2,2,2,2,2,2,2,2,2,4),(0.174342365016846,0.217922519530038,
0.261502674043231,0.305093702038462,0.348684730033692,0.392275758028923,
0.435866786024154,0.479446940537346,0.523027095050539,0.566607249563731,
0.610187404076923,0.653778432072154,0.697369460067385),.UNSPECIFIED.) ;
#417 = B_SPLINE_CURVE_WITH_KNOTS('',3,(#13789,#13790,#13791,#13792,#13793,
#13794,#13795,#13796,#13797,#13798),.UNSPECIFIED.,.F.,.F.,(4,2,2,2,4),(0.,
0.0438474980267263,0.0876949960534527,0.131502815085544,0.175310634117636),
 .UNSPECIFIED.) ;
#418 = B_SPLINE_CURVE_WITH_KNOTS('',3,(#13799,#13800,#13801,#13802,#13803,
#13804,#13805,#13806,#13807,#13808,#13809,#13810,#13811,#13812,#13813,#13814,
#13815,#13816,#13817,#13818,#13819,#13820,#13821,#13822,#13823,#13824),
 .UNSPECIFIED.,.F.,.F.,(4,2,2,2,2,2,2,2,2,2,2,2,4),(0.175310634117636,0.219118453149728,
0.26292627218182,0.306773770208546,0.350621268235272,0.394468766261999,
0.438316264288725,0.482124083320817,0.525931902352908,0.569739721385,0.613547540417092,
0.657395038443818,0.701242536470545),.UNSPECIFIED.) ;
#419 = B_SPLINE_CURVE_WITH_KNOTS('',3,(#14585,#14586,#14587,#14588),
 .UNSPECIFIED.,.F.,.F.,(4,4),(0.941657228299601,0.974745769205032),
 .UNSPECIFIED.) ;
#420 = B_SPLINE_CURVE_WITH_KNOTS('',3,(#14596,#14597,#14598,#14599,#14600,
#14601,#14602,#14603,#14604,#14605),.UNSPECIFIED.,.F.,.F.,(4,2,2,2,4),(0.313885742766534,
0.391923143756541,0.469960544746549,0.548866015139808,0.627771485533068),
 .UNSPECIFIED.) ;
#421 = B_SPLINE_CURVE_WITH_KNOTS('',3,(#14606,#14607,#14608,#14609,#14610,
#14611,#14612,#14613,#14614,#14615),.UNSPECIFIED.,.F.,.F.,(4,2,2,2,4),(0.627771485533068,
0.706676955926327,0.785582426319586,0.863619827309594,0.941657228299601),
 .UNSPECIFIED.) ;
#422 = B_SPLINE_CURVE_WITH_KNOTS('',3,(#14617,#14618,#14619,#14620,#14621,
#14622,#14623,#14624,#14625,#14626,#14627,#14628,#14629,#14630,#14631,#14632,
#14633,#14634,#14635),.UNSPECIFIED.,.F.,.F.,(4,2,2,2,3,2,2,2,4),(0.974745769205032,
1.01969462928961,1.09773203027962,1.17663750067288,1.25554297106614,1.33444844145939,
1.41335391185265,1.49139131284266,1.53634017292724),.UNSPECIFIED.) ;
#423 = B_SPLINE_CURVE_WITH_KNOTS('',3,(#14667,#14668,#14669,#14670),
 .UNSPECIFIED.,.F.,.F.,(4,4),(1.53634017292724,1.56942871383267),
 .UNSPECIFIED.) ;
#424 = B_SPLINE_CURVE_WITH_KNOTS('',3,(#14684,#14685,#14686,#14687,#14688,
#14689,#14690,#14691),.UNSPECIFIED.,.F.,.F.,(4,2,2,4),(0.0875095450662273,
0.155297296869045,0.232550630259834,0.309803963650623),.UNSPECIFIED.) ;
#425 = B_SPLINE_CURVE_WITH_KNOTS('',3,(#14695,#14696,#14697,#14698,#14699,
#14700,#14701,#14702),.UNSPECIFIED.,.F.,.F.,(4,2,2,4),(0.92941189095187,
1.00666522434266,1.08391855773345,1.15170630953627),.UNSPECIFIED.) ;
#426 = B_SPLINE_CURVE_WITH_KNOTS('',3,(#14713,#14714,#14715,#14716,#14717,
#14718,#14719,#14720),.UNSPECIFIED.,.F.,.F.,(4,2,2,4),(0.707117472367471,
0.774905224170291,0.85215855756108,0.92941189095187),.UNSPECIFIED.) ;
#427 = B_SPLINE_CURVE_WITH_KNOTS('',3,(#14723,#14724,#14725,#14726,#14727,
#14728,#14729,#14730),.UNSPECIFIED.,.F.,.F.,(4,2,2,4),(0.309803963650623,
0.387057297041413,0.464310630432203,0.532098382235022),.UNSPECIFIED.) ;
#428 = B_SPLINE_CURVE_WITH_KNOTS('',3,(#14926,#14927,#14928,#14929,#14930,
#14931,#14932,#14933,#14934,#14935,#14936,#14937,#14938,#14939,#14940,#14941,
#14942,#14943),.UNSPECIFIED.,.F.,.F.,(4,2,2,2,2,2,2,2,4),(0.159853073606258,
0.199802153604227,0.239751233602197,0.279728690407356,0.319706147212516,
0.359683604017676,0.399661060822836,0.439610140820805,0.479559220818774),
 .UNSPECIFIED.) ;
#429 = B_SPLINE_CURVE_WITH_KNOTS('',3,(#14944,#14945,#14946,#14947,#14948,
#14949,#14950,#14951,#14952,#14953,#14954,#14955,#14956,#14957,#14958,#14959,
#14960,#14961,#14962),.UNSPECIFIED.,.F.,.F.,(4,2,2,2,3,2,2,2,4),(0.479559220818774,
0.519508300816743,0.559457380814712,0.599434837619873,0.639412294425033,
0.679389751230192,0.719367208035352,0.759316288033321,0.799265368031291),
 .UNSPECIFIED.) ;
#430 = B_SPLINE_CURVE_WITH_KNOTS('',3,(#14966,#14967,#14968,#14969,#14970,
#14971,#14972,#14973,#14974,#14975,#14976,#14977,#14978,#14979,#14980,#14981,
#14982,#14983,#14984),.UNSPECIFIED.,.F.,.F.,(4,2,2,2,3,2,2,2,4),(0.479559220818775,
0.519508300816745,0.559457380814714,0.599434837619874,0.639412294425033,
0.679389751230193,0.719367208035354,0.759316288033323,0.799265368031292),
 .UNSPECIFIED.) ;
#431 = B_SPLINE_CURVE_WITH_KNOTS('',3,(#14985,#14986,#14987,#14988,#14989,
#14990,#14991,#14992,#14993,#14994,#14995,#14996,#14997,#14998,#14999,#15000,
#15001,#15002),.UNSPECIFIED.,.F.,.F.,(4,2,2,2,2,2,2,2,4),(0.159853073606259,
0.199802153604228,0.239751233602197,0.279728690407357,0.319706147212517,
0.359683604017677,0.399661060822836,0.439610140820806,0.479559220818775),
 .UNSPECIFIED.) ;
#432 = B_SPLINE_CURVE_WITH_KNOTS('',3,(#15006,#15007,#15008,#15009,#15010,
#15011,#15012,#15013,#15014,#15015,#15016,#15017,#15018,#15019,#15020,#15021,
#15022,#15023),.UNSPECIFIED.,.F.,.F.,(4,2,2,2,2,2,2,2,4),(0.159853073606258,
0.199802153604227,0.239751233602197,0.279728690407356,0.319706147212516,
0.359683604017676,0.399661060822836,0.439610140820805,0.479559220818774),
 .UNSPECIFIED.) ;
#433 = B_SPLINE_CURVE_WITH_KNOTS('',3,(#15027,#15028,#15029,#15030,#15031,
#15032,#15033,#15034,#15035,#15036,#15037,#15038,#15039,#15040,#15041,#15042,
#15043,#15044),.UNSPECIFIED.,.F.,.F.,(4,2,2,2,2,2,2,2,4),(0.159853073606258,
0.199802153604227,0.239751233602197,0.279728690407356,0.319706147212516,
0.359683604017676,0.399661060822836,0.439610140820805,0.479559220818774),
 .UNSPECIFIED.) ;
#434 = B_SPLINE_CURVE_WITH_KNOTS('',3,(#15045,#15046,#15047,#15048,#15049,
#15050,#15051,#15052,#15053,#15054,#15055,#15056,#15057,#15058,#15059,#15060,
#15061,#15062,#15063),.UNSPECIFIED.,.F.,.F.,(4,2,2,2,3,2,2,2,4),(0.479559220818774,
0.519508300816744,0.559457380814713,0.599434837619873,0.639412294425033,
0.679389751230192,0.719367208035352,0.759316288033321,0.799265368031291),
 .UNSPECIFIED.) ;
#435 = B_SPLINE_CURVE_WITH_KNOTS('',3,(#15064,#15065,#15066,#15067,#15068,
#15069,#15070,#15071,#15072,#15073,#15074,#15075,#15076,#15077,#15078,#15079,
#15080,#15081,#15082),.UNSPECIFIED.,.F.,.F.,(4,2,2,2,3,2,2,2,4),(0.479559220818774,
0.519508300816744,0.559457380814713,0.599434837619873,0.639412294425033,
0.679389751230192,0.719367208035352,0.759316288033321,0.799265368031291),
 .UNSPECIFIED.) ;
#436 = B_SPLINE_CURVE_WITH_KNOTS('',3,(#15304,#15305,#15306,#15307,#15308,
#15309,#15310,#15311,#15312,#15313),.UNSPECIFIED.,.F.,.F.,(4,3,3,4),(-4.09157007060749,
-3.96642934058395,-2.97482200543796,-2.06546402602177),.UNSPECIFIED.) ;
#437 = B_SPLINE_CURVE_WITH_KNOTS('',3,(#15316,#15317,#15318,#15319,#15320,
#15321,#15322),.UNSPECIFIED.,.F.,.F.,(4,3,4),(0.,0.991607335145971,1.11548660900393),
 .UNSPECIFIED.) ;
#438 = B_SPLINE_CURVE_WITH_KNOTS('',3,(#15327,#15328,#15329,#15330,#15331,
#15332,#15333,#15334,#15335,#15336,#15337,#15338,#15339,#15340,#15341,#15342,
#15343,#15344,#15345,#15346,#15347,#15348),.UNSPECIFIED.,.F.,.F.,(4,3,3,
3,3,3,3,4),(-10.3747553777871,-9.91607335145986,-8.92446601631388,-7.93285868116789,
-6.94125134602191,-5.94964401087592,-4.95803667572993,-4.09157007060749),
 .UNSPECIFIED.) ;
#439 = B_SPLINE_CURVE_WITH_KNOTS('',3,(#15349,#15350,#15351,#15352,#15353,
#15354,#15355,#15356,#15357,#15358,#15359,#15360,#15361,#15362,#15363,#15364,
#15365,#15366,#15367,#15368,#15369,#15370),.UNSPECIFIED.,.F.,.F.,(4,3,3,
3,3,3,3,4),(1.11548660900393,1.98321467029196,2.97482200543794,3.96642934058392,
4.95803667572991,5.94964401087589,6.94125134602187,7.39867191618352),
 .UNSPECIFIED.) ;
#440 = B_SPLINE_CURVE_WITH_KNOTS('',3,(#15375,#15376,#15377,#15378,#15379,
#15380,#15381,#15382,#15383,#15384,#15385,#15386,#15387,#15388,#15389,#15390,
#15391,#15392,#15393,#15394,#15395,#15396),.UNSPECIFIED.,.F.,.F.,(4,3,3,
3,3,3,3,4),(-16.6579406849667,-15.8657173623358,-14.8741100271898,-13.8825026920438,
-12.8908953568978,-11.8992880217518,-10.9076806866059,-10.3747553777871),
 .UNSPECIFIED.) ;
#441 = B_SPLINE_CURVE_WITH_KNOTS('',3,(#15397,#15398,#15399,#15400,#15401,
#15402,#15403,#15404,#15405,#15406,#15407,#15408,#15409,#15410,#15411,#15412,
#15413,#15414,#15415,#15416,#15417,#15418),.UNSPECIFIED.,.F.,.F.,(4,3,3,
3,3,3,3,4),(7.39867191618352,7.93285868116786,8.92446601631384,9.91607335145983,
10.9076806866058,11.8992880217518,12.8908953568978,13.6818572233631),
 .UNSPECIFIED.) ;
#442 = B_SPLINE_CURVE_WITH_KNOTS('',3,(#15423,#15424,#15425,#15426,#15427,
#15428,#15429,#15430,#15431,#15432,#15433,#15434,#15435,#15436,#15437,#15438,
#15439,#15440,#15441,#15442,#15443,#15444,#15445,#15446,#15447),
 .UNSPECIFIED.,.F.,.F.,(4,3,3,3,3,3,3,3,4),(-22.9411259921463,-22.8069687083577,
-21.8153613732117,-20.8237540380657,-19.8321467029197,-18.8405393677737,
-17.8489320326278,-16.8573246974818,-16.6579406849667),.UNSPECIFIED.) ;
#443 = B_SPLINE_CURVE_WITH_KNOTS('',3,(#15448,#15449,#15450,#15451,#15452,
#15453,#15454,#15455,#15456,#15457,#15458,#15459,#15460,#15461,#15462,#15463,
#15464,#15465,#15466,#15467,#15468,#15469,#15470,#15471,#15472),
 .UNSPECIFIED.,.F.,.F.,(4,3,3,3,3,3,3,3,4),(13.6818572233631,13.8825026920438,
14.8741100271898,15.8657173623357,16.8573246974817,17.8489320326277,18.8405393677737,
19.8321467029197,19.9650425305427),.UNSPECIFIED.) ;
#444 = B_SPLINE_CURVE_WITH_KNOTS('',3,(#15477,#15478,#15479,#15480,#15481,
#15482,#15483,#15484,#15485,#15486,#15487,#15488,#15489,#15490,#15491,#15492,
#15493,#15494,#15495,#15496,#15497,#15498),.UNSPECIFIED.,.F.,.F.,(4,3,3,
3,3,3,3,4),(-29.2243112993259,-28.7566127192336,-27.7650053840876,-26.7733980489416,
-25.7817907137956,-24.7901833786497,-23.7985760435037,-22.9411259921463),
 .UNSPECIFIED.) ;
#445 = B_SPLINE_CURVE_WITH_KNOTS('',3,(#15499,#15500,#15501,#15502,#15503,
#15504,#15505,#15506,#15507,#15508,#15509,#15510,#15511,#15512,#15513,#15514,
#15515,#15516,#15517,#15518,#15519,#15520),.UNSPECIFIED.,.F.,.F.,(4,3,3,
3,3,3,3,4),(19.9650425305427,20.8237540380657,21.8153613732117,22.8069687083576,
23.7985760435036,24.7901833786496,25.7817907137956,26.2482278377223),
 .UNSPECIFIED.) ;
#446 = B_SPLINE_CURVE_WITH_KNOTS('',3,(#15525,#15526,#15527,#15528,#15529,
#15530,#15531,#15532,#15533,#15534,#15535,#15536,#15537,#15538,#15539,#15540,
#15541,#15542,#15543,#15544,#15545,#15546),.UNSPECIFIED.,.F.,.F.,(4,3,3,
3,3,3,3,4),(-35.5074966065054,-34.7062567301095,-33.7146493949635,-32.7230420598175,
-31.7314347246716,-30.7398273895256,-29.7482200543796,-29.2243112993259),
 .UNSPECIFIED.) ;
#447 = B_SPLINE_CURVE_WITH_KNOTS('',3,(#15547,#15548,#15549,#15550,#15551,
#15552,#15553,#15554,#15555,#15556,#15557,#15558,#15559,#15560,#15561,#15562,
#15563,#15564,#15565,#15566,#15567,#15568),.UNSPECIFIED.,.F.,.F.,(4,3,3,
3,3,3,3,4),(26.2482278377223,26.7733980489416,27.7650053840876,28.7566127192336,
29.7482200543795,30.7398273895255,31.7314347246715,32.5314131449019),
 .UNSPECIFIED.) ;
#448 = B_SPLINE_CURVE_WITH_KNOTS('',3,(#15573,#15574,#15575,#15576,#15577,
#15578,#15579,#15580,#15581,#15582,#15583,#15584,#15585,#15586,#15587,#15588,
#15589,#15590,#15591,#15592,#15593,#15594,#15595,#15596,#15597),
 .UNSPECIFIED.,.F.,.F.,(4,3,3,3,3,3,3,3,4),(-41.790681913685,-41.6475080761314,
-40.6559007409854,-39.6642934058394,-38.6726860706935,-37.6810787355475,
-36.6894714004015,-35.6978640652555,-35.5074966065054),.UNSPECIFIED.) ;
#449 = B_SPLINE_CURVE_WITH_KNOTS('',3,(#15598,#15599,#15600,#15601,#15602,
#15603,#15604,#15605,#15606,#15607,#15608,#15609,#15610,#15611,#15612,#15613,
#15614,#15615,#15616,#15617,#15618,#15619,#15620,#15621,#15622),
 .UNSPECIFIED.,.F.,.F.,(4,3,3,3,3,3,3,3,4),(32.5314131449019,32.7230420598175,
33.7146493949635,34.7062567301095,35.6978640652555,36.6894714004015,37.6810787355474,
38.6726860706934,38.8145984520815),.UNSPECIFIED.) ;
#450 = B_SPLINE_CURVE_WITH_KNOTS('',3,(#15627,#15628,#15629,#15630,#15631,
#15632,#15633,#15634,#15635,#15636,#15637,#15638,#15639,#15640,#15641,#15642,
#15643,#15644,#15645,#15646,#15647,#15648),.UNSPECIFIED.,.F.,.F.,(4,3,3,
3,3,3,3,4),(-48.0738672208646,-47.5971520870073,-46.6055447518613,-45.6139374167154,
-44.6223300815694,-43.6307227464234,-42.6391154112774,-41.790681913685),
 .UNSPECIFIED.) ;
#451 = B_SPLINE_CURVE_WITH_KNOTS('',3,(#15649,#15650,#15651,#15652,#15653,
#15654,#15655,#15656,#15657,#15658,#15659,#15660,#15661,#15662,#15663,#15664,
#15665,#15666,#15667,#15668,#15669,#15670),.UNSPECIFIED.,.F.,.F.,(4,3,3,
3,3,3,3,4),(38.8145984520815,39.6642934058394,40.6559007409854,41.6475080761314,
42.6391154112774,43.6307227464233,44.6223300815693,45.0977837592611),
 .UNSPECIFIED.) ;
#452 = B_SPLINE_CURVE_WITH_KNOTS('',3,(#15675,#15676,#15677,#15678,#15679,
#15680,#15681,#15682,#15683,#15684,#15685,#15686,#15687,#15688,#15689,#15690,
#15691,#15692,#15693,#15694,#15695,#15696),.UNSPECIFIED.,.F.,.F.,(4,3,3,
3,3,3,3,4),(-54.3570525280442,-53.5467960978832,-52.5551887627373,-51.5635814275913,
-50.5719740924453,-49.5803667572993,-48.5887594221533,-48.0738672208646),
 .UNSPECIFIED.) ;
#453 = B_SPLINE_CURVE_WITH_KNOTS('',3,(#15697,#15698,#15699,#15700,#15701,
#15702,#15703,#15704,#15705,#15706,#15707,#15708,#15709,#15710,#15711,#15712,
#15713,#15714,#15715,#15716,#15717,#15718),.UNSPECIFIED.,.F.,.F.,(4,3,3,
3,3,3,3,4),(45.0977837592611,45.6139374167153,46.6055447518613,47.5971520870073,
48.5887594221533,49.5803667572993,50.5719740924452,51.3809690664406),
 .UNSPECIFIED.) ;
#454 = B_SPLINE_CURVE_WITH_KNOTS('',3,(#15723,#15724,#15725,#15726,#15727,
#15728,#15729,#15730,#15731,#15732,#15733,#15734,#15735,#15736,#15737,#15738,
#15739,#15740,#15741,#15742,#15743,#15744,#15745,#15746,#15747),
 .UNSPECIFIED.,.F.,.F.,(4,3,3,3,3,3,3,3,4),(-60.6402378352238,-60.4880474439051,
-59.4964401087592,-58.5048327736132,-57.5132254384672,-56.5216181033212,
-55.5300107681752,-54.5384034330292,-54.3570525280442),.UNSPECIFIED.) ;
#455 = B_SPLINE_CURVE_WITH_KNOTS('',3,(#15748,#15749,#15750,#15751,#15752,
#15753,#15754,#15755,#15756,#15757,#15758,#15759,#15760,#15761,#15762,#15763,
#15764,#15765,#15766,#15767,#15768,#15769,#15770,#15771,#15772),
 .UNSPECIFIED.,.F.,.F.,(4,3,3,3,3,3,3,3,4),(51.3809690664406,51.5635814275912,
52.5551887627372,53.5467960978832,54.5384034330292,55.5300107681752,56.5216181033212,
57.5132254384671,57.6641543736202),.UNSPECIFIED.) ;
#456 = B_SPLINE_CURVE_WITH_KNOTS('',3,(#15777,#15778,#15779,#15780,#15781,
#15782,#15783,#15784,#15785,#15786,#15787,#15788,#15789,#15790,#15791,#15792,
#15793,#15794,#15795,#15796,#15797,#15798),.UNSPECIFIED.,.F.,.F.,(4,3,3,
3,3,3,3,4),(-66.9234231424034,-66.437691454781,-65.4460841196351,-64.4544767844891,
-63.4628694493431,-62.4712621141971,-61.4796547790511,-60.6402378352238),
 .UNSPECIFIED.) ;
#457 = B_SPLINE_CURVE_WITH_KNOTS('',3,(#15799,#15800,#15801,#15802,#15803,
#15804,#15805,#15806,#15807,#15808,#15809,#15810,#15811,#15812,#15813,#15814,
#15815,#15816,#15817,#15818,#15819,#15820),.UNSPECIFIED.,.F.,.F.,(4,3,3,
3,3,3,3,4),(57.6641543736202,58.5048327736131,59.4964401087591,60.4880474439051,
61.4796547790511,62.4712621141971,63.4628694493431,63.9473396807998),
 .UNSPECIFIED.) ;
#458 = B_SPLINE_CURVE_WITH_KNOTS('',3,(#15825,#15826,#15827,#15828,#15829,
#15830,#15831,#15832,#15833,#15834,#15835,#15836,#15837,#15838,#15839,#15840,
#15841,#15842,#15843,#15844,#15845,#15846),.UNSPECIFIED.,.F.,.F.,(4,3,3,
3,3,3,3,4),(-73.206608449583,-72.387335465657,-71.395728130511,-70.404120795365,
-69.412513460219,-68.420906125073,-67.429298789927,-66.9234231424034),
 .UNSPECIFIED.) ;
#459 = B_SPLINE_CURVE_WITH_KNOTS('',3,(#15847,#15848,#15849,#15850,#15851,
#15852,#15853,#15854,#15855,#15856,#15857,#15858,#15859,#15860,#15861,#15862,
#15863,#15864,#15865,#15866,#15867,#15868),.UNSPECIFIED.,.F.,.F.,(4,3,3,
3,3,3,3,4),(63.9473396807998,64.454476784489,65.446084119635,66.437691454781,
67.429298789927,68.420906125073,69.412513460219,70.2305249879794),
 .UNSPECIFIED.) ;
#460 = B_SPLINE_CURVE_WITH_KNOTS('',3,(#15873,#15874,#15875,#15876,#15877,
#15878,#15879,#15880,#15881,#15882,#15883,#15884,#15885,#15886,#15887,#15888,
#15889,#15890,#15891,#15892,#15893,#15894,#15895,#15896,#15897),
 .UNSPECIFIED.,.F.,.F.,(4,3,3,3,3,3,3,3,4),(-79.4897937567626,-79.3285868116789,
-78.3369794765329,-77.3453721413869,-76.3537648062409,-75.3621574710949,
-74.3705501359489,-73.3789428008029,-73.206608449583),.UNSPECIFIED.) ;
#461 = B_SPLINE_CURVE_WITH_KNOTS('',3,(#15898,#15899,#15900,#15901,#15902,
#15903,#15904,#15905,#15906,#15907,#15908,#15909,#15910,#15911,#15912,#15913,
#15914,#15915,#15916,#15917,#15918,#15919,#15920,#15921,#15922),
 .UNSPECIFIED.,.F.,.F.,(4,3,3,3,3,3,3,3,4),(70.2305249879794,70.4041207953649,
71.3957281305109,72.3873354656569,73.3789428008029,74.3705501359489,75.3621574710949,
76.3537648062409,76.513710295159),.UNSPECIFIED.) ;
#462 = B_SPLINE_CURVE_WITH_KNOTS('',3,(#15927,#15928,#15929,#15930,#15931,
#15932,#15933,#15934,#15935,#15936,#15937,#15938,#15939,#15940,#15941,#15942,
#15943,#15944,#15945,#15946,#15947,#15948),.UNSPECIFIED.,.F.,.F.,(4,3,3,
3,3,3,3,4),(-85.7729790639422,-85.2782308225548,-84.2866234874088,-83.2950161522628,
-82.3034088171168,-81.3118014819708,-80.3201941468249,-79.4897937567626),
 .UNSPECIFIED.) ;
#463 = B_SPLINE_CURVE_WITH_KNOTS('',3,(#15949,#15950,#15951,#15952,#15953,
#15954,#15955,#15956,#15957,#15958,#15959,#15960,#15961,#15962,#15963,#15964,
#15965,#15966,#15967,#15968,#15969,#15970),.UNSPECIFIED.,.F.,.F.,(4,3,3,
3,3,3,3,4),(76.513710295159,77.3453721413868,78.3369794765328,79.3285868116788,
80.3201941468248,81.3118014819708,82.3034088171167,82.7968956023386),
 .UNSPECIFIED.) ;
#464 = B_SPLINE_CURVE_WITH_KNOTS('',3,(#15976,#15977,#15978,#15979,#15980),
 .UNSPECIFIED.,.F.,.F.,(4,1,4),(97.3893722612836,97.8862313550422,98.7955893344583),
 .UNSPECIFIED.) ;
#465 = B_SPLINE_CURVE_WITH_KNOTS('',3,(#15983,#15984,#15985,#15986),
 .UNSPECIFIED.,.F.,.F.,(4,4),(97.3893722612836,97.5539515149039),
 .UNSPECIFIED.) ;
#466 = B_SPLINE_CURVE_WITH_KNOTS('',3,(#15991,#15992,#15993,#15994,#15995,
#15996,#15997,#15998,#15999,#16000),.UNSPECIFIED.,.F.,.F.,(4,1,1,1,1,1,
1,4),(91.106186954104,91.9365873441662,92.9281946793122,93.9198020144582,
94.9114093496042,95.9030166847502,96.8946240198962,97.3893722612836),
 .UNSPECIFIED.) ;
#467 = B_SPLINE_CURVE_WITH_KNOTS('',3,(#16001,#16002,#16003,#16004,#16005,
#16006,#16007,#16008,#16009,#16010),.UNSPECIFIED.,.F.,.F.,(4,1,1,1,1,1,
1,4),(91.106186954104,91.604307504028,92.595914839174,93.58752217432,94.579129509466,
95.5707368446119,96.5623441797579,97.3893722612836),.UNSPECIFIED.) ;
#468 = B_SPLINE_CURVE_WITH_KNOTS('',3,(#16015,#16016,#16017,#16018,#16019,
#16020,#16021,#16022,#16023,#16024,#16025),.UNSPECIFIED.,.F.,.F.,(4,1,1,
1,1,1,1,1,4),(84.8230016469244,84.9953359981443,85.9869433332903,86.9785506684363,
87.9701580035823,88.9617653387283,89.9533726738743,90.9449800090203,91.106186954104),
 .UNSPECIFIED.) ;
#469 = B_SPLINE_CURVE_WITH_KNOTS('',3,(#16026,#16027,#16028,#16029,#16030,
#16031,#16032,#16033,#16034,#16035),.UNSPECIFIED.,.F.,.F.,(4,1,1,1,1,1,
1,4),(84.8230016469244,85.6546634931521,86.6462708282981,87.6378781634441,
88.62948549859,89.621092833736,90.612700168882,91.106186954104),
 .UNSPECIFIED.) ;
#470 = B_SPLINE_CURVE_WITH_KNOTS('',3,(#16040,#16041,#16042,#16043,#16044,
#16045,#16046,#16047,#16048,#16049),.UNSPECIFIED.,.F.,.F.,(4,1,1,1,1,1,
1,4),(78.5398163397448,79.0456919872684,80.0372993224144,81.0289066575604,
82.0205139927064,83.0121213278524,84.0037286629984,84.8230016469244),
 .UNSPECIFIED.) ;
#471 = B_SPLINE_CURVE_WITH_KNOTS('',3,(#16050,#16051,#16052,#16053,#16054,
#16055,#16056,#16057,#16058,#16059,#16060),.UNSPECIFIED.,.F.,.F.,(4,1,1,
1,1,1,1,1,4),(78.5398163397448,78.7134121471302,79.7050194822762,80.6966268174222,
81.6882341525682,82.6798414877141,83.6714488228601,84.6630561580061,84.8230016469244),
 .UNSPECIFIED.) ;
#472 = B_SPLINE_CURVE_WITH_KNOTS('',3,(#16065,#16066,#16067,#16068,#16069,
#16070,#16071,#16072,#16073,#16074),.UNSPECIFIED.,.F.,.F.,(4,1,1,1,1,1,
1,4),(72.2566310325652,73.0960479763925,74.0876553115385,75.0792626466845,
76.0708699818305,77.0624773169765,78.0540846521224,78.5398163397448),
 .UNSPECIFIED.) ;
#473 = B_SPLINE_CURVE_WITH_KNOTS('',3,(#16075,#16076,#16077,#16078,#16079,
#16080,#16081,#16082,#16083,#16084),.UNSPECIFIED.,.F.,.F.,(4,1,1,1,1,1,
1,4),(72.2566310325652,72.7637681362543,73.7553754714003,74.7469828065463,
75.7385901416922,76.7301974768382,77.7218048119842,78.5398163397448),
 .UNSPECIFIED.) ;
#474 = B_SPLINE_CURVE_WITH_KNOTS('',3,(#16089,#16090,#16091,#16092,#16093,
#16094,#16095,#16096,#16097,#16098,#16099),.UNSPECIFIED.,.F.,.F.,(4,1,1,
1,1,1,1,1,4),(65.9734457253856,66.1547966303706,67.1464039655166,68.1380113006626,
69.1296186358086,70.1212259709546,71.1128333061005,72.1044406412465,72.2566310325652),
 .UNSPECIFIED.) ;
#475 = B_SPLINE_CURVE_WITH_KNOTS('',3,(#16100,#16101,#16102,#16103,#16104,
#16105,#16106,#16107,#16108,#16109),.UNSPECIFIED.,.F.,.F.,(4,1,1,1,1,1,
1,4),(65.9734457253856,66.8141241253784,67.8057314605244,68.7973387956703,
69.7889461308163,70.7805534659623,71.7721608011083,72.2566310325652),
 .UNSPECIFIED.) ;
#476 = B_SPLINE_CURVE_WITH_KNOTS('',3,(#16114,#16115,#16116,#16117,#16118,
#16119,#16120,#16121,#16122,#16123),.UNSPECIFIED.,.F.,.F.,(4,1,1,1,1,1,
1,4),(59.690260418206,60.2051526194947,61.1967599546407,62.1883672897867,
63.1799746249327,64.1715819600786,65.1631892952246,65.9734457253856),
 .UNSPECIFIED.) ;
#477 = B_SPLINE_CURVE_WITH_KNOTS('',3,(#16124,#16125,#16126,#16127,#16128,
#16129,#16130,#16131,#16132,#16133,#16134),.UNSPECIFIED.,.F.,.F.,(4,1,1,
1,1,1,1,1,4),(59.690260418206,59.8728727793565,60.8644801145025,61.8560874496484,
62.8476947847944,63.8393021199404,64.8309094550864,65.8225167902324,65.9734457253856),
 .UNSPECIFIED.) ;
#478 = B_SPLINE_CURVE_WITH_KNOTS('',3,(#16139,#16140,#16141,#16142,#16143,
#16144,#16145,#16146,#16147,#16148),.UNSPECIFIED.,.F.,.F.,(4,1,1,1,1,1,
1,4),(53.4070751110264,54.2555086086188,55.2471159437648,56.2387232789108,
57.2303306140567,58.2219379492027,59.2135452843487,59.690260418206),
 .UNSPECIFIED.) ;
#479 = B_SPLINE_CURVE_WITH_KNOTS('',3,(#16149,#16150,#16151,#16152,#16153,
#16154,#16155,#16156,#16157,#16158),.UNSPECIFIED.,.F.,.F.,(4,1,1,1,1,1,
1,4),(53.4070751110264,53.9232287684806,54.9148361036265,55.9064434387725,
56.8980507739185,57.8896581090645,58.8812654442105,59.690260418206),
 .UNSPECIFIED.) ;
#480 = B_SPLINE_CURVE_WITH_KNOTS('',3,(#16163,#16164,#16165,#16166,#16167,
#16168,#16169,#16170,#16171,#16172,#16173),.UNSPECIFIED.,.F.,.F.,(4,1,1,
1,1,1,1,1,4),(47.1238898038468,47.3142572625969,48.3058645977429,49.2974719328889,
50.2890792680348,51.2806866031808,52.2722939383268,53.2639012734728,53.4070751110264),
 .UNSPECIFIED.) ;
#481 = B_SPLINE_CURVE_WITH_KNOTS('',3,(#16174,#16175,#16176,#16177,#16178,
#16179,#16180,#16181,#16182,#16183),.UNSPECIFIED.,.F.,.F.,(4,1,1,1,1,1,
1,4),(47.1238898038469,47.9735847576047,48.9651920927506,49.9567994278966,
50.9484067630426,51.9400140981886,52.9316214333346,53.4070751110264),
 .UNSPECIFIED.) ;
#482 = B_SPLINE_CURVE_WITH_KNOTS('',3,(#16188,#16189,#16190,#16191,#16192,
#16193,#16194,#16195,#16196,#16197),.UNSPECIFIED.,.F.,.F.,(4,1,1,1,1,1,
1,4),(40.8407044966673,41.364613251721,42.356220586867,43.3478279220129,
44.3394352571589,45.3310425923049,46.3226499274509,47.1238898038468),
 .UNSPECIFIED.) ;
#483 = B_SPLINE_CURVE_WITH_KNOTS('',3,(#16198,#16199,#16200,#16201,#16202,
#16203,#16204,#16205,#16206,#16207,#16208),.UNSPECIFIED.,.F.,.F.,(4,1,1,
1,1,1,1,1,4),(40.8407044966673,41.0323334115828,42.0239407467287,43.0155480818747,
44.0071554170207,44.9987627521667,45.9903700873127,46.9819774224587,47.1238898038469),
 .UNSPECIFIED.) ;
#484 = B_SPLINE_CURVE_WITH_KNOTS('',3,(#16213,#16214,#16215,#16216,#16217,
#16218,#16219,#16220,#16221,#16222),.UNSPECIFIED.,.F.,.F.,(4,1,1,1,1,1,
1,4),(34.5575191894877,35.4149692408451,36.406576575991,37.398183911137,
38.389791246283,39.381398581429,40.373005916575,40.8407044966673),
 .UNSPECIFIED.) ;
#485 = B_SPLINE_CURVE_WITH_KNOTS('',3,(#16223,#16224,#16225,#16226,#16227,
#16228,#16229,#16230,#16231,#16232),.UNSPECIFIED.,.F.,.F.,(4,1,1,1,1,1,
1,4),(34.5575191894877,35.0826894007068,36.0742967358528,37.0659040709988,
38.0575114061448,39.0491187412908,40.0407260764368,40.8407044966673),
 .UNSPECIFIED.) ;
#486 = B_SPLINE_CURVE_WITH_KNOTS('',3,(#16237,#16238,#16239,#16240,#16241,
#16242,#16243,#16244,#16245,#16246,#16247),.UNSPECIFIED.,.F.,.F.,(4,1,1,
1,1,1,1,1,4),(28.2743338823081,28.4737178948232,29.4653252299691,30.4569325651151,
31.4485399002611,32.4401472354071,33.4317545705531,34.4233619056991,34.5575191894877),
 .UNSPECIFIED.) ;
#487 = B_SPLINE_CURVE_WITH_KNOTS('',3,(#16248,#16249,#16250,#16251,#16252,
#16253,#16254,#16255,#16256,#16257),.UNSPECIFIED.,.F.,.F.,(4,1,1,1,1,1,
1,4),(28.2743338823081,29.1330453898309,30.1246527249769,31.1162600601229,
32.1078673952689,33.0994747304149,34.0910820655609,34.5575191894877),
 .UNSPECIFIED.) ;
#488 = B_SPLINE_CURVE_WITH_KNOTS('',3,(#16262,#16263,#16264,#16265,#16266,
#16267,#16268,#16269,#16270,#16271),.UNSPECIFIED.,.F.,.F.,(4,1,1,1,1,1,
1,4),(21.9911485751285,22.5240738839472,23.5156812190932,24.5072885542392,
25.4988958893852,26.4905032245312,27.4821105596772,28.2743338823081),
 .UNSPECIFIED.) ;
#489 = B_SPLINE_CURVE_WITH_KNOTS('',3,(#16272,#16273,#16274,#16275,#16276,
#16277,#16278,#16279,#16280,#16281,#16282),.UNSPECIFIED.,.F.,.F.,(4,1,1,
1,1,1,1,1,4),(21.9911485751285,22.191794043809,23.183401378955,24.175008714101,
25.166616049247,26.158223384393,27.149830719539,28.1414380546849,28.2743338823081),
 .UNSPECIFIED.) ;
#490 = B_SPLINE_CURVE_WITH_KNOTS('',3,(#16287,#16288,#16289,#16290,#16291,
#16292,#16293,#16294,#16295,#16296),.UNSPECIFIED.,.F.,.F.,(4,1,1,1,1,1,
1,4),(15.7079632679489,16.5744298730713,17.5660372082173,18.5576445433633,
19.5492518785093,20.5408592136553,21.5324665488013,21.9911485751285),
 .UNSPECIFIED.) ;
#491 = B_SPLINE_CURVE_WITH_KNOTS('',3,(#16297,#16298,#16299,#16300,#16301,
#16302,#16303,#16304,#16305,#16306),.UNSPECIFIED.,.F.,.F.,(4,1,1,1,1,1,
1,4),(15.7079632679489,16.2421500329331,17.2337573680791,18.2253647032251,
19.2169720383711,20.2085793735171,21.200186708663,21.9911485751285),
 .UNSPECIFIED.) ;
#492 = B_SPLINE_CURVE_WITH_KNOTS('',3,(#16309,#16310,#16311,#16312,#16313,
#16314,#16315,#16316,#16317,#16318,#16319,#16320,#16321,#16322,#16323,#16324,
#16325,#16326,#16327,#16328,#16329,#16330,#16331,#16332,#16333,#16334,#16335,
#16336,#16337,#16338,#16339,#16340,#16341,#16342,#16343,#16344,#16345,#16346,
#16347,#16348,#16349,#16350,#16351,#16352,#16353,#16354,#16355,#16356,#16357,
#16358,#16359,#16360,#16361,#16362,#16363,#16364,#16365,#16366,#16367,#16368,
#16369,#16370,#16371,#16372,#16373,#16374,#16375,#16376,#16377,#16378,#16379,
#16380,#16381),.UNSPECIFIED.,.F.,.F.,(4,3,3,3,3,3,3,3,3,3,3,3,3,3,3,3,3,
3,3,3,3,3,3,3,4),(-0.178587760439521,-0.172368112300629,-0.16226114537578,
-0.159089326739945,-0.156380108469748,-0.145604887663453,-0.13783812866639,
-0.135347956754248,-0.124003881288268,-0.112570095034531,-0.10661697955651,
-0.103666068884657,-0.0915123769018346,-0.0800733297891053,-0.0748448030148055,
-0.0719656171109528,-0.0694981620716388,-0.0575365254690618,-0.0452971625704305,
-0.0394202376900176,-0.0367681760664848,-0.0343241134637728,-0.0216317222431062,
-0.00902515542907539,0.),.UNSPECIFIED.) ;
#493 = B_SPLINE_CURVE_WITH_KNOTS('',3,(#16386,#16387,#16388,#16389,#16390,
#16391,#16392,#16393,#16394,#16395,#16396,#16397,#16398,#16399,#16400,#16401,
#16402,#16403,#16404,#16405,#16406,#16407,#16408,#16409,#16410,#16411,#16412,
#16413,#16414,#16415,#16416,#16417,#16418,#16419,#16420,#16421,#16422,#16423,
#16424,#16425,#16426,#16427,#16428,#16429,#16430,#16431,#16432,#16433,#16434,
#16435,#16436,#16437,#16438,#16439,#16440,#16441,#16442,#16443,#16444,#16445,
#16446,#16447,#16448,#16449,#16450,#16451,#16452,#16453,#16454,#16455,#16456,
#16457,#16458,#16459,#16460,#16461),.UNSPECIFIED.,.F.,.F.,(4,3,3,3,3,3,
3,3,3,3,3,3,3,3,3,3,3,3,3,3,3,3,3,3,3,4),(-0.177567088092163,-0.169632484827244,
-0.158377014174832,-0.153923063489389,-0.149911964322871,-0.137452002442653,
-0.130219092088315,-0.127499132385944,-0.124937415025536,-0.112988182342971,
-0.101315560244917,-0.0957061865006923,-0.0929123724549286,-0.0906079023280744,
-0.0795887196079492,-0.0692772955064041,-0.0637952726223527,-0.0610743545148113,
-0.0587576989570135,-0.0475705807832961,-0.0365043130610792,-0.0315369939310658,
-0.0291564773895128,-0.0185494534857471,-0.00832706897214829,0.),
 .UNSPECIFIED.) ;
#494 = B_SPLINE_CURVE_WITH_KNOTS('',3,(#16834,#16835,#16836,#16837,#16838,
#16839,#16840,#16841,#16842,#16843,#16844,#16845,#16846,#16847,#16848,#16849),
 .UNSPECIFIED.,.F.,.F.,(4,3,3,3,3,4),(82.7968956023386,83.2950161522627,
84.2866234874087,85.2782308225547,86.2698381577007,87.1791961371168),
 .UNSPECIFIED.) ;
#495 = B_SPLINE_CURVE_WITH_KNOTS('',3,(#16851,#16852,#16853,#16854,#16855,
#16856,#16857,#16858,#16859,#16860,#16861,#16862,#16863,#16864,#16865,#16866,
#16867,#16868,#16869,#16870,#16871,#16872,#16873,#16874,#16875,#16876,#16877,
#16878,#16879,#16880,#16881,#16882,#16883,#16884,#16885,#16886,#16887,#16888,
#16889,#16890,#16891,#16892,#16893,#16894,#16895,#16896,#16897,#16898,#16899,
#16900,#16901,#16902,#16903,#16904,#16905,#16906,#16907,#16908,#16909,#16910,
#16911,#16912,#16913,#16914,#16915,#16916,#16917,#16918,#16919,#16920,#16921,
#16922,#16923),.UNSPECIFIED.,.F.,.F.,(4,3,3,3,3,3,3,3,3,3,3,3,3,3,3,3,3,
3,3,3,3,3,3,3,4),(-0.178587760439465,-0.17236811230058,-0.162261145375735,
-0.159089326536153,-0.156380108199469,-0.145604886686803,-0.137838126692299,
-0.135347954859556,-0.124003879153533,-0.112570093018921,-0.106616976888393,
-0.10366606834618,-0.0915123769018256,-0.0800733297890974,-0.0748448032652592,
-0.0719656187257878,-0.0694981625144281,-0.0575365255268622,-0.0452971622355605,
-0.0394202373519763,-0.0367681765917414,-0.0343241136941139,-0.0216317221625266,
-0.00902515635034675,0.),.UNSPECIFIED.) ;
#496 = B_SPLINE_CURVE_WITH_KNOTS('',3,(#16924,#16925,#16926,#16927,#16928,
#16929,#16930,#16931,#16932),.UNSPECIFIED.,.F.,.F.,(4,1,1,1,1,1,4),(10.374755377787,
11.2841133572032,12.2757206923492,13.2673280274952,14.2589353626411,15.2505426977871,
15.7079632679489),.UNSPECIFIED.) ;
#497 = B_SPLINE_CURVE_WITH_KNOTS('',3,(#16937,#16938,#16939,#16940,#16941,
#16942,#16943,#16944,#16945,#16946,#16947,#16948,#16949,#16950,#16951,#16952,
#16953,#16954,#16955,#16956,#16957,#16958,#16959,#16960,#16961,#16962,#16963,
#16964,#16965,#16966,#16967,#16968,#16969,#16970,#16971,#16972,#16973,#16974,
#16975,#16976,#16977,#16978,#16979,#16980,#16981,#16982,#16983,#16984,#16985,
#16986,#16987,#16988,#16989,#16990,#16991,#16992,#16993,#16994,#16995,#16996,
#16997,#16998,#16999,#17000,#17001,#17002,#17003,#17004,#17005,#17006,#17007,
#17008,#17009,#17010,#17011,#17012),.UNSPECIFIED.,.F.,.F.,(4,3,3,3,3,3,
3,3,3,3,3,3,3,3,3,3,3,3,3,3,3,3,3,3,3,4),(-0.177567088092174,-0.169632484827252,
-0.158377014174843,-0.153923063868584,-0.149911964428064,-0.13745200265245,
-0.130219092271891,-0.127499133676989,-0.124937417107909,-0.11298818500665,
-0.101315564042759,-0.0957061909767678,-0.0929123852241928,-0.0906079053022808,
-0.0795887196079767,-0.069277289277766,-0.0637952645839567,-0.0610743506682683,
-0.0587576970945015,-0.0475705789278521,-0.0365043101748255,-0.0315369900305327,
-0.0291564755179297,-0.0185494505299689,-0.00832706430112883,0.),
 .UNSPECIFIED.) ;
#498 = B_SPLINE_CURVE_WITH_KNOTS('',3,(#17016,#17017,#17018,#17019,#17020,
#17021,#17022,#17023),.UNSPECIFIED.,.F.,.F.,(4,1,1,1,1,4),(11.6163931973414,
12.6080005324874,13.5996078676334,14.5912152027794,15.5828225379253,15.7079632679489),
 .UNSPECIFIED.) ;
#499 = B_SPLINE_CURVE_WITH_KNOTS('',3,(#17396,#17397,#17398,#17399,#17400,
#17401,#17402,#17403,#17404,#17405,#17406,#17407,#17408),.UNSPECIFIED.,
 .F.,.F.,(4,3,3,3,4),(-89.2446601631387,-88.2530528279927,-87.2614454928467,
-86.2698381577008,-85.7729790639422),.UNSPECIFIED.) ;
#500 = CYLINDRICAL_SURFACE('',#9754,1.05) ;
#501 = CYLINDRICAL_SURFACE('',#9761,1.05) ;
#502 = CYLINDRICAL_SURFACE('',#9768,1.05) ;
#503 = CYLINDRICAL_SURFACE('',#9775,1.05) ;
#504 = CYLINDRICAL_SURFACE('',#9779,1.05) ;
#505 = CYLINDRICAL_SURFACE('',#9784,1.05) ;
#506 = CYLINDRICAL_SURFACE('',#9789,1.05) ;
#507 = CYLINDRICAL_SURFACE('',#9793,1.05) ;
#508 = CYLINDRICAL_SURFACE('',#9800,2.05) ;
#509 = CYLINDRICAL_SURFACE('',#9805,2.05) ;
#510 = CYLINDRICAL_SURFACE('',#9809,1.15) ;
#511 = CYLINDRICAL_SURFACE('',#9810,2.95) ;
#512 = CYLINDRICAL_SURFACE('',#9814,1.15) ;
#513 = CYLINDRICAL_SURFACE('',#9815,2.95) ;
#514 = CYLINDRICAL_SURFACE('',#9819,2.05) ;
#515 = CYLINDRICAL_SURFACE('',#9822,2.05) ;
#516 = CYLINDRICAL_SURFACE('',#9825,2.05) ;
#517 = CYLINDRICAL_SURFACE('',#9828,2.05) ;
#518 = CYLINDRICAL_SURFACE('',#9842,3.99999999999999) ;
#519 = CYLINDRICAL_SURFACE('',#9857,3.50000000000001) ;
#520 = CYLINDRICAL_SURFACE('',#9863,3.99999999999999) ;
#521 = CYLINDRICAL_SURFACE('',#9874,3.50000000000001) ;
#522 = CYLINDRICAL_SURFACE('',#9906,2.05) ;
#523 = CYLINDRICAL_SURFACE('',#9909,2.05) ;
#524 = CYLINDRICAL_SURFACE('',#9917,5.00000000000001) ;
#525 = CYLINDRICAL_SURFACE('',#9920,5.00000000000001) ;
#526 = CYLINDRICAL_SURFACE('',#9937,5.00000000000001) ;
#527 = CYLINDRICAL_SURFACE('',#9939,5.00000000000001) ;
#528 = CYLINDRICAL_SURFACE('',#9941,0.5) ;
#529 = CYLINDRICAL_SURFACE('',#9948,0.5) ;
#530 = CYLINDRICAL_SURFACE('',#9954,0.5) ;
#531 = CYLINDRICAL_SURFACE('',#9960,0.5) ;
#532 = CYLINDRICAL_SURFACE('',#9965,6.00000000000001) ;
#533 = CYLINDRICAL_SURFACE('',#9967,6.00000000000001) ;
#534 = CYLINDRICAL_SURFACE('',#9971,5.00000000000001) ;
#535 = CYLINDRICAL_SURFACE('',#9976,5.00000000000001) ;
#536 = CYLINDRICAL_SURFACE('',#9979,6.00000000000001) ;
#537 = CYLINDRICAL_SURFACE('',#9981,6.00000000000001) ;
#538 = CYLINDRICAL_SURFACE('',#9984,2.5) ;
#539 = CYLINDRICAL_SURFACE('',#9987,1.5) ;
#540 = CYLINDRICAL_SURFACE('',#9990,2.05) ;
#541 = CYLINDRICAL_SURFACE('',#9993,2.05) ;
#542 = CYLINDRICAL_SURFACE('',#9997,3.8) ;
#543 = CYLINDRICAL_SURFACE('',#10001,3.8) ;
#544 = CYLINDRICAL_SURFACE('',#10006,1.5) ;
#545 = CYLINDRICAL_SURFACE('',#10009,2.05) ;
#546 = CYLINDRICAL_SURFACE('',#10012,2.05) ;
#547 = CYLINDRICAL_SURFACE('',#10016,3.8) ;
#548 = CYLINDRICAL_SURFACE('',#10020,3.8) ;
#549 = CYLINDRICAL_SURFACE('',#10026,2.5) ;
#550 = CYLINDRICAL_SURFACE('',#10029,2.5) ;
#551 = CYLINDRICAL_SURFACE('',#10032,2.05) ;
#552 = CYLINDRICAL_SURFACE('',#10035,1.5) ;
#553 = CYLINDRICAL_SURFACE('',#10038,2.05) ;
#554 = CYLINDRICAL_SURFACE('',#10042,3.8) ;
#555 = CYLINDRICAL_SURFACE('',#10046,3.8) ;
#556 = CYLINDRICAL_SURFACE('',#10051,1.5) ;
#557 = CYLINDRICAL_SURFACE('',#10054,2.05) ;
#558 = CYLINDRICAL_SURFACE('',#10057,2.05) ;
#559 = CYLINDRICAL_SURFACE('',#10061,3.8) ;
#560 = CYLINDRICAL_SURFACE('',#10065,3.8) ;
#561 = CYLINDRICAL_SURFACE('',#10071,3.) ;
#562 = CYLINDRICAL_SURFACE('',#10073,3.) ;
#563 = CYLINDRICAL_SURFACE('',#10076,2.05) ;
#564 = CYLINDRICAL_SURFACE('',#10081,4.6) ;
#565 = CYLINDRICAL_SURFACE('',#10085,2.09999999999999) ;
#566 = CYLINDRICAL_SURFACE('',#10089,4.99999999999999) ;
#567 = CYLINDRICAL_SURFACE('',#10093,1.99999999999999) ;
#568 = CYLINDRICAL_SURFACE('',#10094,3.) ;
#569 = CYLINDRICAL_SURFACE('',#10099,3.5) ;
#570 = CYLINDRICAL_SURFACE('',#10102,2.55) ;
#571 = CYLINDRICAL_SURFACE('',#10105,3.5) ;
#572 = CYLINDRICAL_SURFACE('',#10115,2.) ;
#573 = CYLINDRICAL_SURFACE('',#10119,4.50000000000001) ;
#574 = CYLINDRICAL_SURFACE('',#10123,2.05) ;
#575 = CYLINDRICAL_SURFACE('',#10143,5.) ;
#576 = CYLINDRICAL_SURFACE('',#10163,2.05) ;
#577 = CYLINDRICAL_SURFACE('',#10165,2.2) ;
#578 = CYLINDRICAL_SURFACE('',#10168,2.19999999999999) ;
#579 = CYLINDRICAL_SURFACE('',#10172,1.05) ;
#580 = CYLINDRICAL_SURFACE('',#10173,1.05) ;
#581 = CYLINDRICAL_SURFACE('',#10174,2.05) ;
#582 = CYLINDRICAL_SURFACE('',#10186,2.85) ;
#583 = CYLINDRICAL_SURFACE('',#10194,2.85) ;
#584 = CYLINDRICAL_SURFACE('',#10201,2.85) ;
#585 = CYLINDRICAL_SURFACE('',#10206,2.05) ;
#586 = CYLINDRICAL_SURFACE('',#10210,2.2) ;
#587 = CYLINDRICAL_SURFACE('',#10214,2.20000000000001) ;
#588 = CYLINDRICAL_SURFACE('',#10224,3.) ;
#589 = CYLINDRICAL_SURFACE('',#10228,2.) ;
#590 = CYLINDRICAL_SURFACE('',#10232,1.59999999999999) ;
#591 = CYLINDRICAL_SURFACE('',#10236,2.) ;
#592 = CYLINDRICAL_SURFACE('',#10246,1.59999999999999) ;
#593 = CYLINDRICAL_SURFACE('',#10251,3.65) ;
#594 = CYLINDRICAL_SURFACE('',#10259,4.) ;
#595 = CYLINDRICAL_SURFACE('',#10265,1.5) ;
#596 = CYLINDRICAL_SURFACE('',#10271,0.96675) ;
#597 = CYLINDRICAL_SURFACE('',#10273,0.96675) ;
#598 = CYLINDRICAL_SURFACE('',#10274,0.96675) ;
#599 = CYLINDRICAL_SURFACE('',#10275,0.96675) ;
#600 = CYLINDRICAL_SURFACE('',#10276,0.96675) ;
#601 = CYLINDRICAL_SURFACE('',#10277,0.96675) ;
#602 = CYLINDRICAL_SURFACE('',#10278,0.96675) ;
#603 = CYLINDRICAL_SURFACE('',#10279,0.96675) ;
#604 = CYLINDRICAL_SURFACE('',#10280,0.96675) ;
#605 = CYLINDRICAL_SURFACE('',#10281,0.96675) ;
#606 = CYLINDRICAL_SURFACE('',#10282,0.96675) ;
#607 = CYLINDRICAL_SURFACE('',#10283,0.96675) ;
#608 = CYLINDRICAL_SURFACE('',#10284,0.96675) ;
#609 = CYLINDRICAL_SURFACE('',#10285,0.96675) ;
#610 = CYLINDRICAL_SURFACE('',#10286,0.739000000000001) ;
#611 = CYLINDRICAL_SURFACE('',#10288,0.739000000000001) ;
#612 = CYLINDRICAL_SURFACE('',#10289,0.739000000000001) ;
#613 = CYLINDRICAL_SURFACE('',#10290,0.739000000000001) ;
#614 = CYLINDRICAL_SURFACE('',#10291,0.739000000000001) ;
#615 = CYLINDRICAL_SURFACE('',#10292,0.739000000000001) ;
#616 = CYLINDRICAL_SURFACE('',#10293,0.739000000000001) ;
#617 = CYLINDRICAL_SURFACE('',#10294,0.739000000000001) ;
#618 = CYLINDRICAL_SURFACE('',#10295,0.739000000000001) ;
#619 = CYLINDRICAL_SURFACE('',#10296,0.739000000000001) ;
#620 = CYLINDRICAL_SURFACE('',#10297,0.739000000000001) ;
#621 = CYLINDRICAL_SURFACE('',#10298,0.739000000000001) ;
#622 = CYLINDRICAL_SURFACE('',#10299,0.739000000000001) ;
#623 = CYLINDRICAL_SURFACE('',#10300,0.739000000000001) ;
#624 = CYLINDRICAL_SURFACE('',#10308,0.739000000000001) ;
#625 = CYLINDRICAL_SURFACE('',#10312,0.96675) ;
#626 = CYLINDRICAL_SURFACE('',#10323,1.9) ;
#627 = CYLINDRICAL_SURFACE('',#10515,0.816025403784444) ;
#628 = CYLINDRICAL_SURFACE('',#10517,0.816025403784444) ;
#629 = CYLINDRICAL_SURFACE('',#10519,0.816025403784444) ;
#630 = CYLINDRICAL_SURFACE('',#10521,0.816025403784444) ;
#631 = CYLINDRICAL_SURFACE('',#10523,0.816025403784444) ;
#632 = CYLINDRICAL_SURFACE('',#10525,0.816025403784444) ;
#633 = CYLINDRICAL_SURFACE('',#10553,1.15) ;
#634 = CYLINDRICAL_SURFACE('',#10556,1.15) ;
#635 = CYLINDRICAL_SURFACE('',#10561,2.04999999999999) ;
#636 = CYLINDRICAL_SURFACE('',#10565,5.) ;
#637 = CYLINDRICAL_SURFACE('',#10578,2.04999999999999) ;
#638 = CYLINDRICAL_SURFACE('',#10581,5.) ;
#639 = CYLINDRICAL_SURFACE('',#10587,4.4) ;
#640 = CYLINDRICAL_SURFACE('',#10591,1.49999999999999) ;
#641 = CYLINDRICAL_SURFACE('',#10600,1.15) ;
#642 = CYLINDRICAL_SURFACE('',#10603,1.15) ;
#643 = CYLINDRICAL_SURFACE('',#10610,2.05) ;
#644 = CYLINDRICAL_SURFACE('',#10613,4.99999999999999) ;
#645 = CYLINDRICAL_SURFACE('',#10620,2.05) ;
#646 = CYLINDRICAL_SURFACE('',#10623,4.99999999999999) ;
#647 = CYLINDRICAL_SURFACE('',#10636,6.00000000000001) ;
#648 = CYLINDRICAL_SURFACE('',#10644,11.65) ;
#649 = CYLINDRICAL_SURFACE('',#10652,6.00000000000001) ;
#650 = CYLINDRICAL_SURFACE('',#10656,2.04999999999999) ;
#651 = FACE_BOUND('',#1608,.T.) ;
#652 = FACE_BOUND('',#1609,.T.) ;
#653 = FACE_BOUND('',#1613,.T.) ;
#654 = FACE_BOUND('',#1614,.T.) ;
#655 = FACE_BOUND('',#1618,.T.) ;
#656 = FACE_BOUND('',#1619,.T.) ;
#657 = FACE_BOUND('',#1623,.T.) ;
#658 = FACE_BOUND('',#1624,.T.) ;
#659 = FACE_BOUND('',#1640,.T.) ;
#660 = FACE_BOUND('',#1644,.T.) ;
#661 = FACE_BOUND('',#1648,.T.) ;
#662 = FACE_BOUND('',#1652,.T.) ;
#663 = FACE_BOUND('',#1660,.T.) ;
#664 = FACE_BOUND('',#1663,.T.) ;
#665 = FACE_BOUND('',#1666,.T.) ;
#666 = FACE_BOUND('',#1670,.T.) ;
#667 = FACE_BOUND('',#1672,.T.) ;
#668 = FACE_BOUND('',#1676,.T.) ;
#669 = FACE_BOUND('',#1678,.T.) ;
#670 = FACE_BOUND('',#1679,.T.) ;
#671 = FACE_BOUND('',#1685,.T.) ;
#672 = FACE_BOUND('',#1690,.T.) ;
#673 = FACE_BOUND('',#1694,.T.) ;
#674 = FACE_BOUND('',#1699,.T.) ;
#675 = FACE_BOUND('',#1714,.T.) ;
#676 = FACE_BOUND('',#1727,.T.) ;
#677 = FACE_BOUND('',#1733,.T.) ;
#678 = FACE_BOUND('',#1738,.T.) ;
#679 = FACE_BOUND('',#1742,.T.) ;
#680 = FACE_BOUND('',#1744,.T.) ;
#681 = FACE_BOUND('',#1747,.T.) ;
#682 = FACE_BOUND('',#1785,.T.) ;
#683 = FACE_BOUND('',#1786,.T.) ;
#684 = FACE_BOUND('',#1787,.T.) ;
#685 = FACE_BOUND('',#1788,.T.) ;
#686 = FACE_BOUND('',#1790,.T.) ;
#687 = FACE_BOUND('',#1791,.T.) ;
#688 = FACE_BOUND('',#1792,.T.) ;
#689 = FACE_BOUND('',#1801,.T.) ;
#690 = FACE_BOUND('',#1802,.T.) ;
#691 = FACE_BOUND('',#1803,.T.) ;
#692 = FACE_BOUND('',#1805,.T.) ;
#693 = FACE_BOUND('',#1806,.T.) ;
#694 = FACE_BOUND('',#1807,.T.) ;
#695 = FACE_BOUND('',#1808,.T.) ;
#696 = FACE_BOUND('',#1819,.T.) ;
#697 = FACE_BOUND('',#1820,.T.) ;
#698 = FACE_BOUND('',#1821,.T.) ;
#699 = FACE_BOUND('',#1822,.T.) ;
#700 = FACE_BOUND('',#1823,.T.) ;
#701 = FACE_BOUND('',#1825,.T.) ;
#702 = FACE_BOUND('',#1826,.T.) ;
#703 = FACE_BOUND('',#1827,.T.) ;
#704 = FACE_BOUND('',#1836,.T.) ;
#705 = FACE_BOUND('',#1837,.T.) ;
#706 = FACE_BOUND('',#1838,.T.) ;
#707 = FACE_BOUND('',#1840,.T.) ;
#708 = FACE_BOUND('',#1841,.T.) ;
#709 = FACE_BOUND('',#1842,.T.) ;
#710 = FACE_BOUND('',#1843,.T.) ;
#711 = FACE_BOUND('',#1844,.T.) ;
#712 = FACE_BOUND('',#1851,.T.) ;
#713 = FACE_BOUND('',#1854,.T.) ;
#714 = FACE_BOUND('',#1857,.T.) ;
#715 = FACE_BOUND('',#1861,.T.) ;
#716 = FACE_BOUND('',#1863,.T.) ;
#717 = FACE_BOUND('',#1868,.T.) ;
#718 = FACE_BOUND('',#1870,.T.) ;
#719 = FACE_BOUND('',#1875,.T.) ;
#720 = FACE_BOUND('',#1903,.T.) ;
#721 = FACE_BOUND('',#1910,.T.) ;
#722 = FACE_BOUND('',#1917,.T.) ;
#723 = FACE_BOUND('',#1920,.T.) ;
#724 = FACE_BOUND('',#1924,.T.) ;
#725 = FACE_BOUND('',#1929,.T.) ;
#726 = FACE_BOUND('',#1930,.T.) ;
#727 = FACE_BOUND('',#1939,.T.) ;
#728 = FACE_BOUND('',#1941,.T.) ;
#729 = FACE_BOUND('',#1946,.T.) ;
#730 = FACE_BOUND('',#1949,.T.) ;
#731 = FACE_BOUND('',#1952,.T.) ;
#732 = FACE_BOUND('',#1969,.T.) ;
#733 = FACE_BOUND('',#2009,.T.) ;
#734 = FACE_BOUND('',#2124,.T.) ;
#735 = FACE_BOUND('',#2159,.T.) ;
#736 = FACE_BOUND('',#2161,.T.) ;
#737 = FACE_BOUND('',#2164,.T.) ;
#738 = FACE_BOUND('',#2171,.T.) ;
#739 = FACE_BOUND('',#2180,.T.) ;
#740 = FACE_BOUND('',#2181,.T.) ;
#741 = FACE_BOUND('',#2182,.T.) ;
#742 = FACE_BOUND('',#2184,.T.) ;
#743 = FACE_BOUND('',#2185,.T.) ;
#744 = FACE_BOUND('',#2186,.T.) ;
#745 = FACE_BOUND('',#2190,.T.) ;
#746 = FACE_BOUND('',#2196,.T.) ;
#747 = FACE_BOUND('',#2198,.T.) ;
#748 = FACE_BOUND('',#2204,.T.) ;
#749 = FACE_BOUND('',#2210,.T.) ;
#750 = FACE_BOUND('',#2211,.T.) ;
#751 = FACE_BOUND('',#2213,.T.) ;
#752 = FACE_BOUND('',#2214,.T.) ;
#753 = FACE_BOUND('',#2215,.T.) ;
#754 = FACE_BOUND('',#2216,.T.) ;
#755 = FACE_BOUND('',#2218,.T.) ;
#756 = FACE_BOUND('',#2221,.T.) ;
#757 = FACE_BOUND('',#2228,.T.) ;
#758 = FACE_BOUND('',#2231,.T.) ;
#759 = PLANE('',#9752) ;
#760 = PLANE('',#9759) ;
#761 = PLANE('',#9766) ;
#762 = PLANE('',#9773) ;
#763 = PLANE('',#9813) ;
#764 = PLANE('',#9818) ;
#765 = PLANE('',#9831) ;
#766 = PLANE('',#9832) ;
#767 = PLANE('',#9834) ;
#768 = PLANE('',#9835) ;
#769 = PLANE('',#9837) ;
#770 = PLANE('',#9838) ;
#771 = PLANE('',#9839) ;
#772 = PLANE('',#9840) ;
#773 = PLANE('',#9841) ;
#774 = PLANE('',#9849) ;
#775 = PLANE('',#9850) ;
#776 = PLANE('',#9851) ;
#777 = PLANE('',#9852) ;
#778 = PLANE('',#9853) ;
#779 = PLANE('',#9855) ;
#780 = PLANE('',#9856) ;
#781 = PLANE('',#9859) ;
#782 = PLANE('',#9860) ;
#783 = PLANE('',#9861) ;
#784 = PLANE('',#9862) ;
#785 = PLANE('',#9869) ;
#786 = PLANE('',#9870) ;
#787 = PLANE('',#9871) ;
#788 = PLANE('',#9872) ;
#789 = PLANE('',#9873) ;
#790 = PLANE('',#9876) ;
#791 = PLANE('',#9877) ;
#792 = PLANE('',#9878) ;
#793 = PLANE('',#9879) ;
#794 = PLANE('',#9880) ;
#795 = PLANE('',#9881) ;
#796 = PLANE('',#9882) ;
#797 = PLANE('',#9883) ;
#798 = PLANE('',#9884) ;
#799 = PLANE('',#9885) ;
#800 = PLANE('',#9886) ;
#801 = PLANE('',#9887) ;
#802 = PLANE('',#9888) ;
#803 = PLANE('',#9889) ;
#804 = PLANE('',#9890) ;
#805 = PLANE('',#9891) ;
#806 = PLANE('',#9892) ;
#807 = PLANE('',#9893) ;
#808 = PLANE('',#9894) ;
#809 = PLANE('',#9895) ;
#810 = PLANE('',#9896) ;
#811 = PLANE('',#9897) ;
#812 = PLANE('',#9898) ;
#813 = PLANE('',#9899) ;
#814 = PLANE('',#9900) ;
#815 = PLANE('',#9901) ;
#816 = PLANE('',#9902) ;
#817 = PLANE('',#9903) ;
#818 = PLANE('',#9904) ;
#819 = PLANE('',#9912) ;
#820 = PLANE('',#9913) ;
#821 = PLANE('',#9914) ;
#822 = PLANE('',#9915) ;
#823 = PLANE('',#9916) ;
#824 = PLANE('',#9923) ;
#825 = PLANE('',#9932) ;
#826 = PLANE('',#9933) ;
#827 = PLANE('',#9934) ;
#828 = PLANE('',#9935) ;
#829 = PLANE('',#9936) ;
#830 = PLANE('',#9966) ;
#831 = PLANE('',#9968) ;
#832 = PLANE('',#9969) ;
#833 = PLANE('',#9970) ;
#834 = PLANE('',#9973) ;
#835 = PLANE('',#9974) ;
#836 = PLANE('',#9975) ;
#837 = PLANE('',#9978) ;
#838 = PLANE('',#9980) ;
#839 = PLANE('',#9982) ;
#840 = PLANE('',#9996) ;
#841 = PLANE('',#10000) ;
#842 = PLANE('',#10004) ;
#843 = PLANE('',#10005) ;
#844 = PLANE('',#10015) ;
#845 = PLANE('',#10019) ;
#846 = PLANE('',#10023) ;
#847 = PLANE('',#10024) ;
#848 = PLANE('',#10041) ;
#849 = PLANE('',#10045) ;
#850 = PLANE('',#10049) ;
#851 = PLANE('',#10050) ;
#852 = PLANE('',#10060) ;
#853 = PLANE('',#10064) ;
#854 = PLANE('',#10068) ;
#855 = PLANE('',#10069) ;
#856 = PLANE('',#10079) ;
#857 = PLANE('',#10083) ;
#858 = PLANE('',#10087) ;
#859 = PLANE('',#10091) ;
#860 = PLANE('',#10096) ;
#861 = PLANE('',#10097) ;
#862 = PLANE('',#10108) ;
#863 = PLANE('',#10109) ;
#864 = PLANE('',#10110) ;
#865 = PLANE('',#10113) ;
#866 = PLANE('',#10117) ;
#867 = PLANE('',#10121) ;
#868 = PLANE('',#10126) ;
#869 = PLANE('',#10127) ;
#870 = PLANE('',#10128) ;
#871 = PLANE('',#10129) ;
#872 = PLANE('',#10131) ;
#873 = PLANE('',#10133) ;
#874 = PLANE('',#10134) ;
#875 = PLANE('',#10135) ;
#876 = PLANE('',#10136) ;
#877 = PLANE('',#10141) ;
#878 = PLANE('',#10146) ;
#879 = PLANE('',#10147) ;
#880 = PLANE('',#10148) ;
#881 = PLANE('',#10149) ;
#882 = PLANE('',#10150) ;
#883 = PLANE('',#10151) ;
#884 = PLANE('',#10153) ;
#885 = PLANE('',#10154) ;
#886 = PLANE('',#10155) ;
#887 = PLANE('',#10156) ;
#888 = PLANE('',#10157) ;
#889 = PLANE('',#10158) ;
#890 = PLANE('',#10162) ;
#891 = PLANE('',#10167) ;
#892 = PLANE('',#10170) ;
#893 = PLANE('',#10177) ;
#894 = PLANE('',#10179) ;
#895 = PLANE('',#10180) ;
#896 = PLANE('',#10181) ;
#897 = PLANE('',#10182) ;
#898 = PLANE('',#10183) ;
#899 = PLANE('',#10184) ;
#900 = PLANE('',#10203) ;
#901 = PLANE('',#10204) ;
#902 = PLANE('',#10209) ;
#903 = PLANE('',#10213) ;
#904 = PLANE('',#10217) ;
#905 = PLANE('',#10218) ;
#906 = PLANE('',#10220) ;
#907 = PLANE('',#10226) ;
#908 = PLANE('',#10230) ;
#909 = PLANE('',#10234) ;
#910 = PLANE('',#10240) ;
#911 = PLANE('',#10242) ;
#912 = PLANE('',#10243) ;
#913 = PLANE('',#10244) ;
#914 = PLANE('',#10245) ;
#915 = PLANE('',#10249) ;
#916 = PLANE('',#10253) ;
#917 = PLANE('',#10255) ;
#918 = PLANE('',#10263) ;
#919 = PLANE('',#10269) ;
#920 = PLANE('',#10301) ;
#921 = PLANE('',#10304) ;
#922 = PLANE('',#10314) ;
#923 = PLANE('',#10318) ;
#924 = PLANE('',#10319) ;
#925 = PLANE('',#10321) ;
#926 = PLANE('',#10322) ;
#927 = PLANE('',#10397) ;
#928 = PLANE('',#10398) ;
#929 = PLANE('',#10399) ;
#930 = PLANE('',#10402) ;
#931 = PLANE('',#10403) ;
#932 = PLANE('',#10404) ;
#933 = PLANE('',#10405) ;
#934 = PLANE('',#10406) ;
#935 = PLANE('',#10407) ;
#936 = PLANE('',#10408) ;
#937 = PLANE('',#10409) ;
#938 = PLANE('',#10410) ;
#939 = PLANE('',#10411) ;
#940 = PLANE('',#10412) ;
#941 = PLANE('',#10413) ;
#942 = PLANE('',#10414) ;
#943 = PLANE('',#10415) ;
#944 = PLANE('',#10416) ;
#945 = PLANE('',#10417) ;
#946 = PLANE('',#10418) ;
#947 = PLANE('',#10419) ;
#948 = PLANE('',#10420) ;
#949 = PLANE('',#10421) ;
#950 = PLANE('',#10422) ;
#951 = PLANE('',#10423) ;
#952 = PLANE('',#10424) ;
#953 = PLANE('',#10425) ;
#954 = PLANE('',#10426) ;
#955 = PLANE('',#10427) ;
#956 = PLANE('',#10428) ;
#957 = PLANE('',#10429) ;
#958 = PLANE('',#10430) ;
#959 = PLANE('',#10431) ;
#960 = PLANE('',#10432) ;
#961 = PLANE('',#10433) ;
#962 = PLANE('',#10434) ;
#963 = PLANE('',#10435) ;
#964 = PLANE('',#10436) ;
#965 = PLANE('',#10437) ;
#966 = PLANE('',#10438) ;
#967 = PLANE('',#10439) ;
#968 = PLANE('',#10440) ;
#969 = PLANE('',#10441) ;
#970 = PLANE('',#10442) ;
#971 = PLANE('',#10443) ;
#972 = PLANE('',#10444) ;
#973 = PLANE('',#10445) ;
#974 = PLANE('',#10446) ;
#975 = PLANE('',#10447) ;
#976 = PLANE('',#10448) ;
#977 = PLANE('',#10449) ;
#978 = PLANE('',#10450) ;
#979 = PLANE('',#10451) ;
#980 = PLANE('',#10452) ;
#981 = PLANE('',#10453) ;
#982 = PLANE('',#10454) ;
#983 = PLANE('',#10455) ;
#984 = PLANE('',#10456) ;
#985 = PLANE('',#10457) ;
#986 = PLANE('',#10458) ;
#987 = PLANE('',#10459) ;
#988 = PLANE('',#10460) ;
#989 = PLANE('',#10461) ;
#990 = PLANE('',#10462) ;
#991 = PLANE('',#10463) ;
#992 = PLANE('',#10464) ;
#993 = PLANE('',#10465) ;
#994 = PLANE('',#10466) ;
#995 = PLANE('',#10467) ;
#996 = PLANE('',#10468) ;
#997 = PLANE('',#10469) ;
#998 = PLANE('',#10470) ;
#999 = PLANE('',#10471) ;
#1000 = PLANE('',#10472) ;
#1001 = PLANE('',#10473) ;
#1002 = PLANE('',#10474) ;
#1003 = PLANE('',#10475) ;
#1004 = PLANE('',#10476) ;
#1005 = PLANE('',#10477) ;
#1006 = PLANE('',#10478) ;
#1007 = PLANE('',#10479) ;
#1008 = PLANE('',#10480) ;
#1009 = PLANE('',#10481) ;
#1010 = PLANE('',#10482) ;
#1011 = PLANE('',#10483) ;
#1012 = PLANE('',#10484) ;
#1013 = PLANE('',#10485) ;
#1014 = PLANE('',#10486) ;
#1015 = PLANE('',#10487) ;
#1016 = PLANE('',#10488) ;
#1017 = PLANE('',#10489) ;
#1018 = PLANE('',#10490) ;
#1019 = PLANE('',#10491) ;
#1020 = PLANE('',#10492) ;
#1021 = PLANE('',#10493) ;
#1022 = PLANE('',#10494) ;
#1023 = PLANE('',#10495) ;
#1024 = PLANE('',#10496) ;
#1025 = PLANE('',#10497) ;
#1026 = PLANE('',#10498) ;
#1027 = PLANE('',#10499) ;
#1028 = PLANE('',#10500) ;
#1029 = PLANE('',#10501) ;
#1030 = PLANE('',#10502) ;
#1031 = PLANE('',#10503) ;
#1032 = PLANE('',#10506) ;
#1033 = PLANE('',#10527) ;
#1034 = PLANE('',#10528) ;
#1035 = PLANE('',#10529) ;
#1036 = PLANE('',#10530) ;
#1037 = PLANE('',#10531) ;
#1038 = PLANE('',#10532) ;
#1039 = PLANE('',#10533) ;
#1040 = PLANE('',#10534) ;
#1041 = PLANE('',#10535) ;
#1042 = PLANE('',#10536) ;
#1043 = PLANE('',#10538) ;
#1044 = PLANE('',#10540) ;
#1045 = PLANE('',#10542) ;
#1046 = PLANE('',#10544) ;
#1047 = PLANE('',#10546) ;
#1048 = PLANE('',#10549) ;
#1049 = PLANE('',#10550) ;
#1050 = PLANE('',#10551) ;
#1051 = PLANE('',#10559) ;
#1052 = PLANE('',#10564) ;
#1053 = PLANE('',#10568) ;
#1054 = PLANE('',#10569) ;
#1055 = PLANE('',#10570) ;
#1056 = PLANE('',#10571) ;
#1057 = PLANE('',#10575) ;
#1058 = PLANE('',#10580) ;
#1059 = PLANE('',#10583) ;
#1060 = PLANE('',#10584) ;
#1061 = PLANE('',#10586) ;
#1062 = PLANE('',#10589) ;
#1063 = PLANE('',#10593) ;
#1064 = PLANE('',#10594) ;
#1065 = PLANE('',#10595) ;
#1066 = PLANE('',#10596) ;
#1067 = PLANE('',#10597) ;
#1068 = PLANE('',#10598) ;
#1069 = PLANE('',#10606) ;
#1070 = PLANE('',#10609) ;
#1071 = PLANE('',#10612) ;
#1072 = PLANE('',#10615) ;
#1073 = PLANE('',#10616) ;
#1074 = PLANE('',#10619) ;
#1075 = PLANE('',#10622) ;
#1076 = PLANE('',#10625) ;
#1077 = PLANE('',#10626) ;
#1078 = PLANE('',#10627) ;
#1079 = PLANE('',#10628) ;
#1080 = PLANE('',#10629) ;
#1081 = PLANE('',#10630) ;
#1082 = PLANE('',#10631) ;
#1083 = PLANE('',#10633) ;
#1084 = PLANE('',#10638) ;
#1085 = PLANE('',#10650) ;
#1086 = PLANE('',#10654) ;
#1087 = FACE_OUTER_BOUND('',#1606,.T.) ;
#1088 = FACE_OUTER_BOUND('',#1607,.T.) ;
#1089 = FACE_OUTER_BOUND('',#1610,.T.) ;
#1090 = FACE_OUTER_BOUND('',#1611,.T.) ;
#1091 = FACE_OUTER_BOUND('',#1612,.T.) ;
#1092 = FACE_OUTER_BOUND('',#1615,.T.) ;
#1093 = FACE_OUTER_BOUND('',#1616,.T.) ;
#1094 = FACE_OUTER_BOUND('',#1617,.T.) ;
#1095 = FACE_OUTER_BOUND('',#1620,.T.) ;
#1096 = FACE_OUTER_BOUND('',#1621,.T.) ;
#1097 = FACE_OUTER_BOUND('',#1622,.T.) ;
#1098 = FACE_OUTER_BOUND('',#1625,.T.) ;
#1099 = FACE_OUTER_BOUND('',#1626,.T.) ;
#1100 = FACE_OUTER_BOUND('',#1627,.T.) ;
#1101 = FACE_OUTER_BOUND('',#1628,.T.) ;
#1102 = FACE_OUTER_BOUND('',#1629,.T.) ;
#1103 = FACE_OUTER_BOUND('',#1630,.T.) ;
#1104 = FACE_OUTER_BOUND('',#1631,.T.) ;
#1105 = FACE_OUTER_BOUND('',#1632,.T.) ;
#1106 = FACE_OUTER_BOUND('',#1633,.T.) ;
#1107 = FACE_OUTER_BOUND('',#1634,.T.) ;
#1108 = FACE_OUTER_BOUND('',#1635,.T.) ;
#1109 = FACE_OUTER_BOUND('',#1636,.T.) ;
#1110 = FACE_OUTER_BOUND('',#1637,.T.) ;
#1111 = FACE_OUTER_BOUND('',#1638,.T.) ;
#1112 = FACE_OUTER_BOUND('',#1639,.T.) ;
#1113 = FACE_OUTER_BOUND('',#1641,.T.) ;
#1114 = FACE_OUTER_BOUND('',#1642,.T.) ;
#1115 = FACE_OUTER_BOUND('',#1643,.T.) ;
#1116 = FACE_OUTER_BOUND('',#1645,.T.) ;
#1117 = FACE_OUTER_BOUND('',#1646,.T.) ;
#1118 = FACE_OUTER_BOUND('',#1647,.T.) ;
#1119 = FACE_OUTER_BOUND('',#1649,.T.) ;
#1120 = FACE_OUTER_BOUND('',#1650,.T.) ;
#1121 = FACE_OUTER_BOUND('',#1651,.T.) ;
#1122 = FACE_OUTER_BOUND('',#1653,.T.) ;
#1123 = FACE_OUTER_BOUND('',#1654,.T.) ;
#1124 = FACE_OUTER_BOUND('',#1655,.T.) ;
#1125 = FACE_OUTER_BOUND('',#1656,.T.) ;
#1126 = FACE_OUTER_BOUND('',#1657,.T.) ;
#1127 = FACE_OUTER_BOUND('',#1658,.T.) ;
#1128 = FACE_OUTER_BOUND('',#1659,.T.) ;
#1129 = FACE_OUTER_BOUND('',#1661,.T.) ;
#1130 = FACE_OUTER_BOUND('',#1662,.T.) ;
#1131 = FACE_OUTER_BOUND('',#1664,.T.) ;
#1132 = FACE_OUTER_BOUND('',#1665,.T.) ;
#1133 = FACE_OUTER_BOUND('',#1667,.T.) ;
#1134 = FACE_OUTER_BOUND('',#1668,.T.) ;
#1135 = FACE_OUTER_BOUND('',#1669,.T.) ;
#1136 = FACE_OUTER_BOUND('',#1671,.T.) ;
#1137 = FACE_OUTER_BOUND('',#1673,.T.) ;
#1138 = FACE_OUTER_BOUND('',#1674,.T.) ;
#1139 = FACE_OUTER_BOUND('',#1675,.T.) ;
#1140 = FACE_OUTER_BOUND('',#1677,.T.) ;
#1141 = FACE_OUTER_BOUND('',#1680,.T.) ;
#1142 = FACE_OUTER_BOUND('',#1681,.T.) ;
#1143 = FACE_OUTER_BOUND('',#1682,.T.) ;
#1144 = FACE_OUTER_BOUND('',#1683,.T.) ;
#1145 = FACE_OUTER_BOUND('',#1684,.T.) ;
#1146 = FACE_OUTER_BOUND('',#1686,.T.) ;
#1147 = FACE_OUTER_BOUND('',#1687,.T.) ;
#1148 = FACE_OUTER_BOUND('',#1688,.T.) ;
#1149 = FACE_OUTER_BOUND('',#1689,.T.) ;
#1150 = FACE_OUTER_BOUND('',#1691,.T.) ;
#1151 = FACE_OUTER_BOUND('',#1692,.T.) ;
#1152 = FACE_OUTER_BOUND('',#1693,.T.) ;
#1153 = FACE_OUTER_BOUND('',#1695,.T.) ;
#1154 = FACE_OUTER_BOUND('',#1696,.T.) ;
#1155 = FACE_OUTER_BOUND('',#1697,.T.) ;
#1156 = FACE_OUTER_BOUND('',#1698,.T.) ;
#1157 = FACE_OUTER_BOUND('',#1700,.T.) ;
#1158 = FACE_OUTER_BOUND('',#1701,.T.) ;
#1159 = FACE_OUTER_BOUND('',#1702,.T.) ;
#1160 = FACE_OUTER_BOUND('',#1703,.T.) ;
#1161 = FACE_OUTER_BOUND('',#1704,.T.) ;
#1162 = FACE_OUTER_BOUND('',#1705,.T.) ;
#1163 = FACE_OUTER_BOUND('',#1706,.T.) ;
#1164 = FACE_OUTER_BOUND('',#1707,.T.) ;
#1165 = FACE_OUTER_BOUND('',#1708,.T.) ;
#1166 = FACE_OUTER_BOUND('',#1709,.T.) ;
#1167 = FACE_OUTER_BOUND('',#1710,.T.) ;
#1168 = FACE_OUTER_BOUND('',#1711,.T.) ;
#1169 = FACE_OUTER_BOUND('',#1712,.T.) ;
#1170 = FACE_OUTER_BOUND('',#1713,.T.) ;
#1171 = FACE_OUTER_BOUND('',#1715,.T.) ;
#1172 = FACE_OUTER_BOUND('',#1716,.T.) ;
#1173 = FACE_OUTER_BOUND('',#1717,.T.) ;
#1174 = FACE_OUTER_BOUND('',#1718,.T.) ;
#1175 = FACE_OUTER_BOUND('',#1719,.T.) ;
#1176 = FACE_OUTER_BOUND('',#1720,.T.) ;
#1177 = FACE_OUTER_BOUND('',#1721,.T.) ;
#1178 = FACE_OUTER_BOUND('',#1722,.T.) ;
#1179 = FACE_OUTER_BOUND('',#1723,.T.) ;
#1180 = FACE_OUTER_BOUND('',#1724,.T.) ;
#1181 = FACE_OUTER_BOUND('',#1725,.T.) ;
#1182 = FACE_OUTER_BOUND('',#1726,.T.) ;
#1183 = FACE_OUTER_BOUND('',#1728,.T.) ;
#1184 = FACE_OUTER_BOUND('',#1729,.T.) ;
#1185 = FACE_OUTER_BOUND('',#1730,.T.) ;
#1186 = FACE_OUTER_BOUND('',#1731,.T.) ;
#1187 = FACE_OUTER_BOUND('',#1732,.T.) ;
#1188 = FACE_OUTER_BOUND('',#1734,.T.) ;
#1189 = FACE_OUTER_BOUND('',#1735,.T.) ;
#1190 = FACE_OUTER_BOUND('',#1736,.T.) ;
#1191 = FACE_OUTER_BOUND('',#1737,.T.) ;
#1192 = FACE_OUTER_BOUND('',#1739,.T.) ;
#1193 = FACE_OUTER_BOUND('',#1740,.T.) ;
#1194 = FACE_OUTER_BOUND('',#1741,.T.) ;
#1195 = FACE_OUTER_BOUND('',#1743,.T.) ;
#1196 = FACE_OUTER_BOUND('',#1745,.T.) ;
#1197 = FACE_OUTER_BOUND('',#1746,.T.) ;
#1198 = FACE_OUTER_BOUND('',#1748,.T.) ;
#1199 = FACE_OUTER_BOUND('',#1749,.T.) ;
#1200 = FACE_OUTER_BOUND('',#1750,.T.) ;
#1201 = FACE_OUTER_BOUND('',#1751,.T.) ;
#1202 = FACE_OUTER_BOUND('',#1752,.T.) ;
#1203 = FACE_OUTER_BOUND('',#1753,.T.) ;
#1204 = FACE_OUTER_BOUND('',#1754,.T.) ;
#1205 = FACE_OUTER_BOUND('',#1755,.T.) ;
#1206 = FACE_OUTER_BOUND('',#1756,.T.) ;
#1207 = FACE_OUTER_BOUND('',#1757,.T.) ;
#1208 = FACE_OUTER_BOUND('',#1758,.T.) ;
#1209 = FACE_OUTER_BOUND('',#1759,.T.) ;
#1210 = FACE_OUTER_BOUND('',#1760,.T.) ;
#1211 = FACE_OUTER_BOUND('',#1761,.T.) ;
#1212 = FACE_OUTER_BOUND('',#1762,.T.) ;
#1213 = FACE_OUTER_BOUND('',#1763,.T.) ;
#1214 = FACE_OUTER_BOUND('',#1764,.T.) ;
#1215 = FACE_OUTER_BOUND('',#1765,.T.) ;
#1216 = FACE_OUTER_BOUND('',#1766,.T.) ;
#1217 = FACE_OUTER_BOUND('',#1767,.T.) ;
#1218 = FACE_OUTER_BOUND('',#1768,.T.) ;
#1219 = FACE_OUTER_BOUND('',#1769,.T.) ;
#1220 = FACE_OUTER_BOUND('',#1770,.T.) ;
#1221 = FACE_OUTER_BOUND('',#1771,.T.) ;
#1222 = FACE_OUTER_BOUND('',#1772,.T.) ;
#1223 = FACE_OUTER_BOUND('',#1773,.T.) ;
#1224 = FACE_OUTER_BOUND('',#1774,.T.) ;
#1225 = FACE_OUTER_BOUND('',#1775,.T.) ;
#1226 = FACE_OUTER_BOUND('',#1776,.T.) ;
#1227 = FACE_OUTER_BOUND('',#1777,.T.) ;
#1228 = FACE_OUTER_BOUND('',#1778,.T.) ;
#1229 = FACE_OUTER_BOUND('',#1779,.T.) ;
#1230 = FACE_OUTER_BOUND('',#1780,.T.) ;
#1231 = FACE_OUTER_BOUND('',#1781,.T.) ;
#1232 = FACE_OUTER_BOUND('',#1782,.T.) ;
#1233 = FACE_OUTER_BOUND('',#1783,.T.) ;
#1234 = FACE_OUTER_BOUND('',#1784,.T.) ;
#1235 = FACE_OUTER_BOUND('',#1789,.T.) ;
#1236 = FACE_OUTER_BOUND('',#1793,.T.) ;
#1237 = FACE_OUTER_BOUND('',#1794,.T.) ;
#1238 = FACE_OUTER_BOUND('',#1795,.T.) ;
#1239 = FACE_OUTER_BOUND('',#1796,.T.) ;
#1240 = FACE_OUTER_BOUND('',#1797,.T.) ;
#1241 = FACE_OUTER_BOUND('',#1798,.T.) ;
#1242 = FACE_OUTER_BOUND('',#1799,.T.) ;
#1243 = FACE_OUTER_BOUND('',#1800,.T.) ;
#1244 = FACE_OUTER_BOUND('',#1804,.T.) ;
#1245 = FACE_OUTER_BOUND('',#1809,.T.) ;
#1246 = FACE_OUTER_BOUND('',#1810,.T.) ;
#1247 = FACE_OUTER_BOUND('',#1811,.T.) ;
#1248 = FACE_OUTER_BOUND('',#1812,.T.) ;
#1249 = FACE_OUTER_BOUND('',#1813,.T.) ;
#1250 = FACE_OUTER_BOUND('',#1814,.T.) ;
#1251 = FACE_OUTER_BOUND('',#1815,.T.) ;
#1252 = FACE_OUTER_BOUND('',#1816,.T.) ;
#1253 = FACE_OUTER_BOUND('',#1817,.T.) ;
#1254 = FACE_OUTER_BOUND('',#1818,.T.) ;
#1255 = FACE_OUTER_BOUND('',#1824,.T.) ;
#1256 = FACE_OUTER_BOUND('',#1828,.T.) ;
#1257 = FACE_OUTER_BOUND('',#1829,.T.) ;
#1258 = FACE_OUTER_BOUND('',#1830,.T.) ;
#1259 = FACE_OUTER_BOUND('',#1831,.T.) ;
#1260 = FACE_OUTER_BOUND('',#1832,.T.) ;
#1261 = FACE_OUTER_BOUND('',#1833,.T.) ;
#1262 = FACE_OUTER_BOUND('',#1834,.T.) ;
#1263 = FACE_OUTER_BOUND('',#1835,.T.) ;
#1264 = FACE_OUTER_BOUND('',#1839,.T.) ;
#1265 = FACE_OUTER_BOUND('',#1845,.T.) ;
#1266 = FACE_OUTER_BOUND('',#1846,.T.) ;
#1267 = FACE_OUTER_BOUND('',#1847,.T.) ;
#1268 = FACE_OUTER_BOUND('',#1848,.T.) ;
#1269 = FACE_OUTER_BOUND('',#1849,.T.) ;
#1270 = FACE_OUTER_BOUND('',#1850,.T.) ;
#1271 = FACE_OUTER_BOUND('',#1852,.T.) ;
#1272 = FACE_OUTER_BOUND('',#1853,.T.) ;
#1273 = FACE_OUTER_BOUND('',#1855,.T.) ;
#1274 = FACE_OUTER_BOUND('',#1856,.T.) ;
#1275 = FACE_OUTER_BOUND('',#1858,.T.) ;
#1276 = FACE_OUTER_BOUND('',#1859,.T.) ;
#1277 = FACE_OUTER_BOUND('',#1860,.T.) ;
#1278 = FACE_OUTER_BOUND('',#1862,.T.) ;
#1279 = FACE_OUTER_BOUND('',#1864,.T.) ;
#1280 = FACE_OUTER_BOUND('',#1865,.T.) ;
#1281 = FACE_OUTER_BOUND('',#1866,.T.) ;
#1282 = FACE_OUTER_BOUND('',#1867,.T.) ;
#1283 = FACE_OUTER_BOUND('',#1869,.T.) ;
#1284 = FACE_OUTER_BOUND('',#1871,.T.) ;
#1285 = FACE_OUTER_BOUND('',#1872,.T.) ;
#1286 = FACE_OUTER_BOUND('',#1873,.T.) ;
#1287 = FACE_OUTER_BOUND('',#1874,.T.) ;
#1288 = FACE_OUTER_BOUND('',#1876,.T.) ;
#1289 = FACE_OUTER_BOUND('',#1877,.T.) ;
#1290 = FACE_OUTER_BOUND('',#1878,.T.) ;
#1291 = FACE_OUTER_BOUND('',#1879,.T.) ;
#1292 = FACE_OUTER_BOUND('',#1880,.T.) ;
#1293 = FACE_OUTER_BOUND('',#1881,.T.) ;
#1294 = FACE_OUTER_BOUND('',#1882,.T.) ;
#1295 = FACE_OUTER_BOUND('',#1883,.T.) ;
#1296 = FACE_OUTER_BOUND('',#1884,.T.) ;
#1297 = FACE_OUTER_BOUND('',#1885,.T.) ;
#1298 = FACE_OUTER_BOUND('',#1886,.T.) ;
#1299 = FACE_OUTER_BOUND('',#1887,.T.) ;
#1300 = FACE_OUTER_BOUND('',#1888,.T.) ;
#1301 = FACE_OUTER_BOUND('',#1889,.T.) ;
#1302 = FACE_OUTER_BOUND('',#1890,.T.) ;
#1303 = FACE_OUTER_BOUND('',#1891,.T.) ;
#1304 = FACE_OUTER_BOUND('',#1892,.T.) ;
#1305 = FACE_OUTER_BOUND('',#1893,.T.) ;
#1306 = FACE_OUTER_BOUND('',#1894,.T.) ;
#1307 = FACE_OUTER_BOUND('',#1895,.T.) ;
#1308 = FACE_OUTER_BOUND('',#1896,.T.) ;
#1309 = FACE_OUTER_BOUND('',#1897,.T.) ;
#1310 = FACE_OUTER_BOUND('',#1898,.T.) ;
#1311 = FACE_OUTER_BOUND('',#1899,.T.) ;
#1312 = FACE_OUTER_BOUND('',#1900,.T.) ;
#1313 = FACE_OUTER_BOUND('',#1901,.T.) ;
#1314 = FACE_OUTER_BOUND('',#1902,.T.) ;
#1315 = FACE_OUTER_BOUND('',#1904,.T.) ;
#1316 = FACE_OUTER_BOUND('',#1905,.T.) ;
#1317 = FACE_OUTER_BOUND('',#1906,.T.) ;
#1318 = FACE_OUTER_BOUND('',#1907,.T.) ;
#1319 = FACE_OUTER_BOUND('',#1908,.T.) ;
#1320 = FACE_OUTER_BOUND('',#1909,.T.) ;
#1321 = FACE_OUTER_BOUND('',#1911,.T.) ;
#1322 = FACE_OUTER_BOUND('',#1912,.T.) ;
#1323 = FACE_OUTER_BOUND('',#1913,.T.) ;
#1324 = FACE_OUTER_BOUND('',#1914,.T.) ;
#1325 = FACE_OUTER_BOUND('',#1915,.T.) ;
#1326 = FACE_OUTER_BOUND('',#1916,.T.) ;
#1327 = FACE_OUTER_BOUND('',#1918,.T.) ;
#1328 = FACE_OUTER_BOUND('',#1919,.T.) ;
#1329 = FACE_OUTER_BOUND('',#1921,.T.) ;
#1330 = FACE_OUTER_BOUND('',#1922,.T.) ;
#1331 = FACE_OUTER_BOUND('',#1923,.T.) ;
#1332 = FACE_OUTER_BOUND('',#1925,.T.) ;
#1333 = FACE_OUTER_BOUND('',#1926,.T.) ;
#1334 = FACE_OUTER_BOUND('',#1927,.T.) ;
#1335 = FACE_OUTER_BOUND('',#1928,.T.) ;
#1336 = FACE_OUTER_BOUND('',#1931,.T.) ;
#1337 = FACE_OUTER_BOUND('',#1932,.T.) ;
#1338 = FACE_OUTER_BOUND('',#1933,.T.) ;
#1339 = FACE_OUTER_BOUND('',#1934,.T.) ;
#1340 = FACE_OUTER_BOUND('',#1935,.T.) ;
#1341 = FACE_OUTER_BOUND('',#1936,.T.) ;
#1342 = FACE_OUTER_BOUND('',#1937,.T.) ;
#1343 = FACE_OUTER_BOUND('',#1938,.T.) ;
#1344 = FACE_OUTER_BOUND('',#1940,.T.) ;
#1345 = FACE_OUTER_BOUND('',#1942,.T.) ;
#1346 = FACE_OUTER_BOUND('',#1943,.T.) ;
#1347 = FACE_OUTER_BOUND('',#1944,.T.) ;
#1348 = FACE_OUTER_BOUND('',#1945,.T.) ;
#1349 = FACE_OUTER_BOUND('',#1947,.T.) ;
#1350 = FACE_OUTER_BOUND('',#1948,.T.) ;
#1351 = FACE_OUTER_BOUND('',#1950,.T.) ;
#1352 = FACE_OUTER_BOUND('',#1951,.T.) ;
#1353 = FACE_OUTER_BOUND('',#1953,.T.) ;
#1354 = FACE_OUTER_BOUND('',#1954,.T.) ;
#1355 = FACE_OUTER_BOUND('',#1955,.T.) ;
#1356 = FACE_OUTER_BOUND('',#1956,.T.) ;
#1357 = FACE_OUTER_BOUND('',#1957,.T.) ;
#1358 = FACE_OUTER_BOUND('',#1958,.T.) ;
#1359 = FACE_OUTER_BOUND('',#1959,.T.) ;
#1360 = FACE_OUTER_BOUND('',#1960,.T.) ;
#1361 = FACE_OUTER_BOUND('',#1961,.T.) ;
#1362 = FACE_OUTER_BOUND('',#1962,.T.) ;
#1363 = FACE_OUTER_BOUND('',#1963,.T.) ;
#1364 = FACE_OUTER_BOUND('',#1964,.T.) ;
#1365 = FACE_OUTER_BOUND('',#1965,.T.) ;
#1366 = FACE_OUTER_BOUND('',#1966,.T.) ;
#1367 = FACE_OUTER_BOUND('',#1967,.T.) ;
#1368 = FACE_OUTER_BOUND('',#1968,.T.) ;
#1369 = FACE_OUTER_BOUND('',#1970,.T.) ;
#1370 = FACE_OUTER_BOUND('',#1971,.T.) ;
#1371 = FACE_OUTER_BOUND('',#1972,.T.) ;
#1372 = FACE_OUTER_BOUND('',#1973,.T.) ;
#1373 = FACE_OUTER_BOUND('',#1974,.T.) ;
#1374 = FACE_OUTER_BOUND('',#1975,.T.) ;
#1375 = FACE_OUTER_BOUND('',#1976,.T.) ;
#1376 = FACE_OUTER_BOUND('',#1977,.T.) ;
#1377 = FACE_OUTER_BOUND('',#1978,.T.) ;
#1378 = FACE_OUTER_BOUND('',#1979,.T.) ;
#1379 = FACE_OUTER_BOUND('',#1980,.T.) ;
#1380 = FACE_OUTER_BOUND('',#1981,.T.) ;
#1381 = FACE_OUTER_BOUND('',#1982,.T.) ;
#1382 = FACE_OUTER_BOUND('',#1983,.T.) ;
#1383 = FACE_OUTER_BOUND('',#1984,.T.) ;
#1384 = FACE_OUTER_BOUND('',#1985,.T.) ;
#1385 = FACE_OUTER_BOUND('',#1986,.T.) ;
#1386 = FACE_OUTER_BOUND('',#1987,.T.) ;
#1387 = FACE_OUTER_BOUND('',#1988,.T.) ;
#1388 = FACE_OUTER_BOUND('',#1989,.T.) ;
#1389 = FACE_OUTER_BOUND('',#1990,.T.) ;
#1390 = FACE_OUTER_BOUND('',#1991,.T.) ;
#1391 = FACE_OUTER_BOUND('',#1992,.T.) ;
#1392 = FACE_OUTER_BOUND('',#1993,.T.) ;
#1393 = FACE_OUTER_BOUND('',#1994,.T.) ;
#1394 = FACE_OUTER_BOUND('',#1995,.T.) ;
#1395 = FACE_OUTER_BOUND('',#1996,.T.) ;
#1396 = FACE_OUTER_BOUND('',#1997,.T.) ;
#1397 = FACE_OUTER_BOUND('',#1998,.T.) ;
#1398 = FACE_OUTER_BOUND('',#1999,.T.) ;
#1399 = FACE_OUTER_BOUND('',#2000,.T.) ;
#1400 = FACE_OUTER_BOUND('',#2001,.T.) ;
#1401 = FACE_OUTER_BOUND('',#2002,.T.) ;
#1402 = FACE_OUTER_BOUND('',#2003,.T.) ;
#1403 = FACE_OUTER_BOUND('',#2004,.T.) ;
#1404 = FACE_OUTER_BOUND('',#2005,.T.) ;
#1405 = FACE_OUTER_BOUND('',#2006,.T.) ;
#1406 = FACE_OUTER_BOUND('',#2007,.T.) ;
#1407 = FACE_OUTER_BOUND('',#2008,.T.) ;
#1408 = FACE_OUTER_BOUND('',#2010,.T.) ;
#1409 = FACE_OUTER_BOUND('',#2011,.T.) ;
#1410 = FACE_OUTER_BOUND('',#2012,.T.) ;
#1411 = FACE_OUTER_BOUND('',#2013,.T.) ;
#1412 = FACE_OUTER_BOUND('',#2014,.T.) ;
#1413 = FACE_OUTER_BOUND('',#2015,.T.) ;
#1414 = FACE_OUTER_BOUND('',#2016,.T.) ;
#1415 = FACE_OUTER_BOUND('',#2017,.T.) ;
#1416 = FACE_OUTER_BOUND('',#2018,.T.) ;
#1417 = FACE_OUTER_BOUND('',#2019,.T.) ;
#1418 = FACE_OUTER_BOUND('',#2020,.T.) ;
#1419 = FACE_OUTER_BOUND('',#2021,.T.) ;
#1420 = FACE_OUTER_BOUND('',#2022,.T.) ;
#1421 = FACE_OUTER_BOUND('',#2023,.T.) ;
#1422 = FACE_OUTER_BOUND('',#2024,.T.) ;
#1423 = FACE_OUTER_BOUND('',#2025,.T.) ;
#1424 = FACE_OUTER_BOUND('',#2026,.T.) ;
#1425 = FACE_OUTER_BOUND('',#2027,.T.) ;
#1426 = FACE_OUTER_BOUND('',#2028,.T.) ;
#1427 = FACE_OUTER_BOUND('',#2029,.T.) ;
#1428 = FACE_OUTER_BOUND('',#2030,.T.) ;
#1429 = FACE_OUTER_BOUND('',#2031,.T.) ;
#1430 = FACE_OUTER_BOUND('',#2032,.T.) ;
#1431 = FACE_OUTER_BOUND('',#2033,.T.) ;
#1432 = FACE_OUTER_BOUND('',#2034,.T.) ;
#1433 = FACE_OUTER_BOUND('',#2035,.T.) ;
#1434 = FACE_OUTER_BOUND('',#2036,.T.) ;
#1435 = FACE_OUTER_BOUND('',#2037,.T.) ;
#1436 = FACE_OUTER_BOUND('',#2038,.T.) ;
#1437 = FACE_OUTER_BOUND('',#2039,.T.) ;
#1438 = FACE_OUTER_BOUND('',#2040,.T.) ;
#1439 = FACE_OUTER_BOUND('',#2041,.T.) ;
#1440 = FACE_OUTER_BOUND('',#2042,.T.) ;
#1441 = FACE_OUTER_BOUND('',#2043,.T.) ;
#1442 = FACE_OUTER_BOUND('',#2044,.T.) ;
#1443 = FACE_OUTER_BOUND('',#2045,.T.) ;
#1444 = FACE_OUTER_BOUND('',#2046,.T.) ;
#1445 = FACE_OUTER_BOUND('',#2047,.T.) ;
#1446 = FACE_OUTER_BOUND('',#2048,.T.) ;
#1447 = FACE_OUTER_BOUND('',#2049,.T.) ;
#1448 = FACE_OUTER_BOUND('',#2050,.T.) ;
#1449 = FACE_OUTER_BOUND('',#2051,.T.) ;
#1450 = FACE_OUTER_BOUND('',#2052,.T.) ;
#1451 = FACE_OUTER_BOUND('',#2053,.T.) ;
#1452 = FACE_OUTER_BOUND('',#2054,.T.) ;
#1453 = FACE_OUTER_BOUND('',#2055,.T.) ;
#1454 = FACE_OUTER_BOUND('',#2056,.T.) ;
#1455 = FACE_OUTER_BOUND('',#2057,.T.) ;
#1456 = FACE_OUTER_BOUND('',#2058,.T.) ;
#1457 = FACE_OUTER_BOUND('',#2059,.T.) ;
#1458 = FACE_OUTER_BOUND('',#2060,.T.) ;
#1459 = FACE_OUTER_BOUND('',#2061,.T.) ;
#1460 = FACE_OUTER_BOUND('',#2062,.T.) ;
#1461 = FACE_OUTER_BOUND('',#2063,.T.) ;
#1462 = FACE_OUTER_BOUND('',#2064,.T.) ;
#1463 = FACE_OUTER_BOUND('',#2065,.T.) ;
#1464 = FACE_OUTER_BOUND('',#2066,.T.) ;
#1465 = FACE_OUTER_BOUND('',#2067,.T.) ;
#1466 = FACE_OUTER_BOUND('',#2068,.T.) ;
#1467 = FACE_OUTER_BOUND('',#2069,.T.) ;
#1468 = FACE_OUTER_BOUND('',#2070,.T.) ;
#1469 = FACE_OUTER_BOUND('',#2071,.T.) ;
#1470 = FACE_OUTER_BOUND('',#2072,.T.) ;
#1471 = FACE_OUTER_BOUND('',#2073,.T.) ;
#1472 = FACE_OUTER_BOUND('',#2074,.T.) ;
#1473 = FACE_OUTER_BOUND('',#2075,.T.) ;
#1474 = FACE_OUTER_BOUND('',#2076,.T.) ;
#1475 = FACE_OUTER_BOUND('',#2077,.T.) ;
#1476 = FACE_OUTER_BOUND('',#2078,.T.) ;
#1477 = FACE_OUTER_BOUND('',#2079,.T.) ;
#1478 = FACE_OUTER_BOUND('',#2080,.T.) ;
#1479 = FACE_OUTER_BOUND('',#2081,.T.) ;
#1480 = FACE_OUTER_BOUND('',#2082,.T.) ;
#1481 = FACE_OUTER_BOUND('',#2083,.T.) ;
#1482 = FACE_OUTER_BOUND('',#2084,.T.) ;
#1483 = FACE_OUTER_BOUND('',#2085,.T.) ;
#1484 = FACE_OUTER_BOUND('',#2086,.T.) ;
#1485 = FACE_OUTER_BOUND('',#2087,.T.) ;
#1486 = FACE_OUTER_BOUND('',#2088,.T.) ;
#1487 = FACE_OUTER_BOUND('',#2089,.T.) ;
#1488 = FACE_OUTER_BOUND('',#2090,.T.) ;
#1489 = FACE_OUTER_BOUND('',#2091,.T.) ;
#1490 = FACE_OUTER_BOUND('',#2092,.T.) ;
#1491 = FACE_OUTER_BOUND('',#2093,.T.) ;
#1492 = FACE_OUTER_BOUND('',#2094,.T.) ;
#1493 = FACE_OUTER_BOUND('',#2095,.T.) ;
#1494 = FACE_OUTER_BOUND('',#2096,.T.) ;
#1495 = FACE_OUTER_BOUND('',#2097,.T.) ;
#1496 = FACE_OUTER_BOUND('',#2098,.T.) ;
#1497 = FACE_OUTER_BOUND('',#2099,.T.) ;
#1498 = FACE_OUTER_BOUND('',#2100,.T.) ;
#1499 = FACE_OUTER_BOUND('',#2101,.T.) ;
#1500 = FACE_OUTER_BOUND('',#2102,.T.) ;
#1501 = FACE_OUTER_BOUND('',#2103,.T.) ;
#1502 = FACE_OUTER_BOUND('',#2104,.T.) ;
#1503 = FACE_OUTER_BOUND('',#2105,.T.) ;
#1504 = FACE_OUTER_BOUND('',#2106,.T.) ;
#1505 = FACE_OUTER_BOUND('',#2107,.T.) ;
#1506 = FACE_OUTER_BOUND('',#2108,.T.) ;
#1507 = FACE_OUTER_BOUND('',#2109,.T.) ;
#1508 = FACE_OUTER_BOUND('',#2110,.T.) ;
#1509 = FACE_OUTER_BOUND('',#2111,.T.) ;
#1510 = FACE_OUTER_BOUND('',#2112,.T.) ;
#1511 = FACE_OUTER_BOUND('',#2113,.T.) ;
#1512 = FACE_OUTER_BOUND('',#2114,.T.) ;
#1513 = FACE_OUTER_BOUND('',#2115,.T.) ;
#1514 = FACE_OUTER_BOUND('',#2116,.T.) ;
#1515 = FACE_OUTER_BOUND('',#2117,.T.) ;
#1516 = FACE_OUTER_BOUND('',#2118,.T.) ;
#1517 = FACE_OUTER_BOUND('',#2119,.T.) ;
#1518 = FACE_OUTER_BOUND('',#2120,.T.) ;
#1519 = FACE_OUTER_BOUND('',#2121,.T.) ;
#1520 = FACE_OUTER_BOUND('',#2122,.T.) ;
#1521 = FACE_OUTER_BOUND('',#2123,.T.) ;
#1522 = FACE_OUTER_BOUND('',#2125,.T.) ;
#1523 = FACE_OUTER_BOUND('',#2126,.T.) ;
#1524 = FACE_OUTER_BOUND('',#2127,.T.) ;
#1525 = FACE_OUTER_BOUND('',#2128,.T.) ;
#1526 = FACE_OUTER_BOUND('',#2129,.T.) ;
#1527 = FACE_OUTER_BOUND('',#2130,.T.) ;
#1528 = FACE_OUTER_BOUND('',#2131,.T.) ;
#1529 = FACE_OUTER_BOUND('',#2132,.T.) ;
#1530 = FACE_OUTER_BOUND('',#2133,.T.) ;
#1531 = FACE_OUTER_BOUND('',#2134,.T.) ;
#1532 = FACE_OUTER_BOUND('',#2135,.T.) ;
#1533 = FACE_OUTER_BOUND('',#2136,.T.) ;
#1534 = FACE_OUTER_BOUND('',#2137,.T.) ;
#1535 = FACE_OUTER_BOUND('',#2138,.T.) ;
#1536 = FACE_OUTER_BOUND('',#2139,.T.) ;
#1537 = FACE_OUTER_BOUND('',#2140,.T.) ;
#1538 = FACE_OUTER_BOUND('',#2141,.T.) ;
#1539 = FACE_OUTER_BOUND('',#2142,.T.) ;
#1540 = FACE_OUTER_BOUND('',#2143,.T.) ;
#1541 = FACE_OUTER_BOUND('',#2144,.T.) ;
#1542 = FACE_OUTER_BOUND('',#2145,.T.) ;
#1543 = FACE_OUTER_BOUND('',#2146,.T.) ;
#1544 = FACE_OUTER_BOUND('',#2147,.T.) ;
#1545 = FACE_OUTER_BOUND('',#2148,.T.) ;
#1546 = FACE_OUTER_BOUND('',#2149,.T.) ;
#1547 = FACE_OUTER_BOUND('',#2150,.T.) ;
#1548 = FACE_OUTER_BOUND('',#2151,.T.) ;
#1549 = FACE_OUTER_BOUND('',#2152,.T.) ;
#1550 = FACE_OUTER_BOUND('',#2153,.T.) ;
#1551 = FACE_OUTER_BOUND('',#2154,.T.) ;
#1552 = FACE_OUTER_BOUND('',#2155,.T.) ;
#1553 = FACE_OUTER_BOUND('',#2156,.T.) ;
#1554 = FACE_OUTER_BOUND('',#2157,.T.) ;
#1555 = FACE_OUTER_BOUND('',#2158,.T.) ;
#1556 = FACE_OUTER_BOUND('',#2160,.T.) ;
#1557 = FACE_OUTER_BOUND('',#2162,.T.) ;
#1558 = FACE_OUTER_BOUND('',#2163,.T.) ;
#1559 = FACE_OUTER_BOUND('',#2165,.T.) ;
#1560 = FACE_OUTER_BOUND('',#2166,.T.) ;
#1561 = FACE_OUTER_BOUND('',#2167,.T.) ;
#1562 = FACE_OUTER_BOUND('',#2168,.T.) ;
#1563 = FACE_OUTER_BOUND('',#2169,.T.) ;
#1564 = FACE_OUTER_BOUND('',#2170,.T.) ;
#1565 = FACE_OUTER_BOUND('',#2172,.T.) ;
#1566 = FACE_OUTER_BOUND('',#2173,.T.) ;
#1567 = FACE_OUTER_BOUND('',#2174,.T.) ;
#1568 = FACE_OUTER_BOUND('',#2175,.T.) ;
#1569 = FACE_OUTER_BOUND('',#2176,.T.) ;
#1570 = FACE_OUTER_BOUND('',#2177,.T.) ;
#1571 = FACE_OUTER_BOUND('',#2178,.T.) ;
#1572 = FACE_OUTER_BOUND('',#2179,.T.) ;
#1573 = FACE_OUTER_BOUND('',#2183,.T.) ;
#1574 = FACE_OUTER_BOUND('',#2187,.T.) ;
#1575 = FACE_OUTER_BOUND('',#2188,.T.) ;
#1576 = FACE_OUTER_BOUND('',#2189,.T.) ;
#1577 = FACE_OUTER_BOUND('',#2191,.T.) ;
#1578 = FACE_OUTER_BOUND('',#2192,.T.) ;
#1579 = FACE_OUTER_BOUND('',#2193,.T.) ;
#1580 = FACE_OUTER_BOUND('',#2194,.T.) ;
#1581 = FACE_OUTER_BOUND('',#2195,.T.) ;
#1582 = FACE_OUTER_BOUND('',#2197,.T.) ;
#1583 = FACE_OUTER_BOUND('',#2199,.T.) ;
#1584 = FACE_OUTER_BOUND('',#2200,.T.) ;
#1585 = FACE_OUTER_BOUND('',#2201,.T.) ;
#1586 = FACE_OUTER_BOUND('',#2202,.T.) ;
#1587 = FACE_OUTER_BOUND('',#2203,.T.) ;
#1588 = FACE_OUTER_BOUND('',#2205,.T.) ;
#1589 = FACE_OUTER_BOUND('',#2206,.T.) ;
#1590 = FACE_OUTER_BOUND('',#2207,.T.) ;
#1591 = FACE_OUTER_BOUND('',#2208,.T.) ;
#1592 = FACE_OUTER_BOUND('',#2209,.T.) ;
#1593 = FACE_OUTER_BOUND('',#2212,.T.) ;
#1594 = FACE_OUTER_BOUND('',#2217,.T.) ;
#1595 = FACE_OUTER_BOUND('',#2219,.T.) ;
#1596 = FACE_OUTER_BOUND('',#2220,.T.) ;
#1597 = FACE_OUTER_BOUND('',#2222,.T.) ;
#1598 = FACE_OUTER_BOUND('',#2223,.T.) ;
#1599 = FACE_OUTER_BOUND('',#2224,.T.) ;
#1600 = FACE_OUTER_BOUND('',#2225,.T.) ;
#1601 = FACE_OUTER_BOUND('',#2226,.T.) ;
#1602 = FACE_OUTER_BOUND('',#2227,.T.) ;
#1603 = FACE_OUTER_BOUND('',#2229,.T.) ;
#1604 = FACE_OUTER_BOUND('',#2230,.T.) ;
#1605 = FACE_OUTER_BOUND('',#2232,.T.) ;
#1606 = EDGE_LOOP('',(#6343,#6344,#6345,#6346)) ;
#1607 = EDGE_LOOP('',(#6347,#6348,#6349,#6350)) ;
#1608 = EDGE_LOOP('',(#6351)) ;
#1609 = EDGE_LOOP('',(#6352)) ;
#1610 = EDGE_LOOP('',(#6353,#6354,#6355,#6356)) ;
#1611 = EDGE_LOOP('',(#6357,#6358,#6359,#6360)) ;
#1612 = EDGE_LOOP('',(#6361,#6362,#6363,#6364)) ;
#1613 = EDGE_LOOP('',(#6365)) ;
#1614 = EDGE_LOOP('',(#6366)) ;
#1615 = EDGE_LOOP('',(#6367,#6368,#6369,#6370)) ;
#1616 = EDGE_LOOP('',(#6371,#6372,#6373,#6374)) ;
#1617 = EDGE_LOOP('',(#6375,#6376,#6377,#6378)) ;
#1618 = EDGE_LOOP('',(#6379)) ;
#1619 = EDGE_LOOP('',(#6380)) ;
#1620 = EDGE_LOOP('',(#6381,#6382,#6383,#6384)) ;
#1621 = EDGE_LOOP('',(#6385,#6386,#6387,#6388)) ;
#1622 = EDGE_LOOP('',(#6389,#6390,#6391,#6392)) ;
#1623 = EDGE_LOOP('',(#6393)) ;
#1624 = EDGE_LOOP('',(#6394)) ;
#1625 = EDGE_LOOP('',(#6395,#6396,#6397,#6398)) ;
#1626 = EDGE_LOOP('',(#6399,#6400,#6401,#6402)) ;
#1627 = EDGE_LOOP('',(#6403,#6404,#6405,#6406,#6407,#6408)) ;
#1628 = EDGE_LOOP('',(#6409,#6410,#6411,#6412)) ;
#1629 = EDGE_LOOP('',(#6413,#6414,#6415,#6416,#6417,#6418)) ;
#1630 = EDGE_LOOP('',(#6419,#6420,#6421,#6422)) ;
#1631 = EDGE_LOOP('',(#6423,#6424,#6425,#6426)) ;
#1632 = EDGE_LOOP('',(#6427,#6428,#6429,#6430)) ;
#1633 = EDGE_LOOP('',(#6431,#6432,#6433,#6434)) ;
#1634 = EDGE_LOOP('',(#6435,#6436,#6437)) ;
#1635 = EDGE_LOOP('',(#6438,#6439,#6440)) ;
#1636 = EDGE_LOOP('',(#6441,#6442,#6443)) ;
#1637 = EDGE_LOOP('',(#6444,#6445,#6446)) ;
#1638 = EDGE_LOOP('',(#6447,#6448,#6449)) ;
#1639 = EDGE_LOOP('',(#6450,#6451,#6452,#6453)) ;
#1640 = EDGE_LOOP('',(#6454,#6455)) ;
#1641 = EDGE_LOOP('',(#6456,#6457,#6458)) ;
#1642 = EDGE_LOOP('',(#6459,#6460,#6461)) ;
#1643 = EDGE_LOOP('',(#6462,#6463,#6464,#6465)) ;
#1644 = EDGE_LOOP('',(#6466,#6467)) ;
#1645 = EDGE_LOOP('',(#6468,#6469,#6470)) ;
#1646 = EDGE_LOOP('',(#6471,#6472,#6473,#6474,#6475,#6476)) ;
#1647 = EDGE_LOOP('',(#6477,#6478,#6479,#6480)) ;
#1648 = EDGE_LOOP('',(#6481,#6482)) ;
#1649 = EDGE_LOOP('',(#6483)) ;
#1650 = EDGE_LOOP('',(#6484,#6485,#6486,#6487,#6488,#6489)) ;
#1651 = EDGE_LOOP('',(#6490,#6491,#6492,#6493)) ;
#1652 = EDGE_LOOP('',(#6494,#6495)) ;
#1653 = EDGE_LOOP('',(#6496)) ;
#1654 = EDGE_LOOP('',(#6497,#6498,#6499,#6500)) ;
#1655 = EDGE_LOOP('',(#6501,#6502,#6503,#6504)) ;
#1656 = EDGE_LOOP('',(#6505,#6506,#6507,#6508)) ;
#1657 = EDGE_LOOP('',(#6509,#6510,#6511,#6512)) ;
#1658 = EDGE_LOOP('',(#6513,#6514,#6515,#6516)) ;
#1659 = EDGE_LOOP('',(#6517,#6518,#6519,#6520,#6521,#6522)) ;
#1660 = EDGE_LOOP('',(#6523)) ;
#1661 = EDGE_LOOP('',(#6524,#6525,#6526,#6527)) ;
#1662 = EDGE_LOOP('',(#6528,#6529,#6530,#6531,#6532,#6533)) ;
#1663 = EDGE_LOOP('',(#6534)) ;
#1664 = EDGE_LOOP('',(#6535,#6536,#6537,#6538)) ;
#1665 = EDGE_LOOP('',(#6539,#6540,#6541,#6542,#6543,#6544)) ;
#1666 = EDGE_LOOP('',(#6545)) ;
#1667 = EDGE_LOOP('',(#6546,#6547,#6548,#6549,#6550,#6551,#6552,#6553,#6554,
#6555,#6556,#6557,#6558,#6559,#6560,#6561,#6562,#6563,#6564,#6565,#6566,
#6567)) ;
#1668 = EDGE_LOOP('',(#6568,#6569,#6570,#6571)) ;
#1669 = EDGE_LOOP('',(#6572,#6573,#6574,#6575,#6576,#6577)) ;
#1670 = EDGE_LOOP('',(#6578)) ;
#1671 = EDGE_LOOP('',(#6579,#6580,#6581,#6582,#6583,#6584,#6585,#6586,#6587,
#6588,#6589,#6590)) ;
#1672 = EDGE_LOOP('',(#6591,#6592)) ;
#1673 = EDGE_LOOP('',(#6593,#6594)) ;
#1674 = EDGE_LOOP('',(#6595,#6596,#6597)) ;
#1675 = EDGE_LOOP('',(#6598)) ;
#1676 = EDGE_LOOP('',(#6599)) ;
#1677 = EDGE_LOOP('',(#6600,#6601,#6602,#6603,#6604,#6605,#6606,#6607,#6608,
#6609,#6610,#6611,#6612,#6613)) ;
#1678 = EDGE_LOOP('',(#6614,#6615,#6616,#6617)) ;
#1679 = EDGE_LOOP('',(#6618,#6619,#6620,#6621)) ;
#1680 = EDGE_LOOP('',(#6622,#6623,#6624,#6625)) ;
#1681 = EDGE_LOOP('',(#6626,#6627,#6628,#6629)) ;
#1682 = EDGE_LOOP('',(#6630,#6631,#6632,#6633)) ;
#1683 = EDGE_LOOP('',(#6634,#6635,#6636,#6637)) ;
#1684 = EDGE_LOOP('',(#6638,#6639,#6640,#6641,#6642,#6643)) ;
#1685 = EDGE_LOOP('',(#6644)) ;
#1686 = EDGE_LOOP('',(#6645,#6646,#6647,#6648)) ;
#1687 = EDGE_LOOP('',(#6649,#6650,#6651,#6652)) ;
#1688 = EDGE_LOOP('',(#6653,#6654,#6655,#6656)) ;
#1689 = EDGE_LOOP('',(#6657,#6658,#6659,#6660,#6661,#6662,#6663,#6664,#6665,
#6666,#6667,#6668)) ;
#1690 = EDGE_LOOP('',(#6669,#6670)) ;
#1691 = EDGE_LOOP('',(#6671,#6672)) ;
#1692 = EDGE_LOOP('',(#6673,#6674,#6675)) ;
#1693 = EDGE_LOOP('',(#6676)) ;
#1694 = EDGE_LOOP('',(#6677)) ;
#1695 = EDGE_LOOP('',(#6678,#6679,#6680,#6681)) ;
#1696 = EDGE_LOOP('',(#6682,#6683,#6684,#6685)) ;
#1697 = EDGE_LOOP('',(#6686,#6687,#6688,#6689)) ;
#1698 = EDGE_LOOP('',(#6690,#6691,#6692,#6693,#6694,#6695)) ;
#1699 = EDGE_LOOP('',(#6696)) ;
#1700 = EDGE_LOOP('',(#6697,#6698,#6699,#6700)) ;
#1701 = EDGE_LOOP('',(#6701,#6702,#6703,#6704)) ;
#1702 = EDGE_LOOP('',(#6705,#6706,#6707,#6708)) ;
#1703 = EDGE_LOOP('',(#6709,#6710,#6711,#6712)) ;
#1704 = EDGE_LOOP('',(#6713,#6714,#6715,#6716)) ;
#1705 = EDGE_LOOP('',(#6717,#6718,#6719,#6720,#6721)) ;
#1706 = EDGE_LOOP('',(#6722,#6723,#6724,#6725)) ;
#1707 = EDGE_LOOP('',(#6726,#6727,#6728,#6729)) ;
#1708 = EDGE_LOOP('',(#6730,#6731,#6732,#6733)) ;
#1709 = EDGE_LOOP('',(#6734,#6735,#6736,#6737,#6738)) ;
#1710 = EDGE_LOOP('',(#6739,#6740,#6741,#6742)) ;
#1711 = EDGE_LOOP('',(#6743,#6744,#6745,#6746,#6747,#6748,#6749,#6750,#6751,
#6752,#6753,#6754,#6755,#6756,#6757,#6758)) ;
#1712 = EDGE_LOOP('',(#6759,#6760,#6761,#6762,#6763,#6764,#6765,#6766)) ;
#1713 = EDGE_LOOP('',(#6767,#6768,#6769,#6770,#6771,#6772,#6773)) ;
#1714 = EDGE_LOOP('',(#6774)) ;
#1715 = EDGE_LOOP('',(#6775,#6776,#6777,#6778)) ;
#1716 = EDGE_LOOP('',(#6779,#6780,#6781,#6782,#6783)) ;
#1717 = EDGE_LOOP('',(#6784,#6785,#6786,#6787)) ;
#1718 = EDGE_LOOP('',(#6788,#6789,#6790,#6791,#6792,#6793)) ;
#1719 = EDGE_LOOP('',(#6794,#6795,#6796,#6797)) ;
#1720 = EDGE_LOOP('',(#6798,#6799,#6800,#6801)) ;
#1721 = EDGE_LOOP('',(#6802,#6803,#6804,#6805)) ;
#1722 = EDGE_LOOP('',(#6806,#6807,#6808,#6809)) ;
#1723 = EDGE_LOOP('',(#6810,#6811,#6812,#6813)) ;
#1724 = EDGE_LOOP('',(#6814,#6815,#6816,#6817,#6818)) ;
#1725 = EDGE_LOOP('',(#6819,#6820,#6821,#6822,#6823,#6824)) ;
#1726 = EDGE_LOOP('',(#6825,#6826,#6827,#6828,#6829,#6830,#6831)) ;
#1727 = EDGE_LOOP('',(#6832)) ;
#1728 = EDGE_LOOP('',(#6833,#6834,#6835,#6836,#6837,#6838,#6839,#6840,#6841,
#6842,#6843,#6844,#6845,#6846)) ;
#1729 = EDGE_LOOP('',(#6847,#6848,#6849,#6850,#6851,#6852,#6853,#6854,#6855,
#6856,#6857,#6858)) ;
#1730 = EDGE_LOOP('',(#6859,#6860,#6861,#6862)) ;
#1731 = EDGE_LOOP('',(#6863,#6864,#6865,#6866)) ;
#1732 = EDGE_LOOP('',(#6867,#6868,#6869,#6870)) ;
#1733 = EDGE_LOOP('',(#6871)) ;
#1734 = EDGE_LOOP('',(#6872,#6873,#6874,#6875,#6876,#6877)) ;
#1735 = EDGE_LOOP('',(#6878,#6879,#6880,#6881)) ;
#1736 = EDGE_LOOP('',(#6882,#6883,#6884,#6885)) ;
#1737 = EDGE_LOOP('',(#6886,#6887,#6888,#6889,#6890,#6891)) ;
#1738 = EDGE_LOOP('',(#6892)) ;
#1739 = EDGE_LOOP('',(#6893,#6894,#6895,#6896)) ;
#1740 = EDGE_LOOP('',(#6897,#6898,#6899,#6900)) ;
#1741 = EDGE_LOOP('',(#6901,#6902,#6903,#6904,#6905,#6906,#6907,#6908)) ;
#1742 = EDGE_LOOP('',(#6909,#6910,#6911,#6912,#6913,#6914,#6915,#6916,#6917,
#6918,#6919,#6920,#6921,#6922)) ;
#1743 = EDGE_LOOP('',(#6923,#6924,#6925,#6926)) ;
#1744 = EDGE_LOOP('',(#6927)) ;
#1745 = EDGE_LOOP('',(#6928,#6929,#6930,#6931)) ;
#1746 = EDGE_LOOP('',(#6932,#6933,#6934,#6935,#6936,#6937)) ;
#1747 = EDGE_LOOP('',(#6938)) ;
#1748 = EDGE_LOOP('',(#6939,#6940,#6941,#6942)) ;
#1749 = EDGE_LOOP('',(#6943,#6944,#6945,#6946,#6947,#6948)) ;
#1750 = EDGE_LOOP('',(#6949,#6950,#6951,#6952)) ;
#1751 = EDGE_LOOP('',(#6953,#6954,#6955,#6956)) ;
#1752 = EDGE_LOOP('',(#6957,#6958,#6959,#6960)) ;
#1753 = EDGE_LOOP('',(#6961,#6962,#6963,#6964)) ;
#1754 = EDGE_LOOP('',(#6965,#6966,#6967,#6968)) ;
#1755 = EDGE_LOOP('',(#6969,#6970,#6971,#6972)) ;
#1756 = EDGE_LOOP('',(#6973,#6974,#6975,#6976)) ;
#1757 = EDGE_LOOP('',(#6977,#6978,#6979,#6980)) ;
#1758 = EDGE_LOOP('',(#6981,#6982,#6983,#6984)) ;
#1759 = EDGE_LOOP('',(#6985,#6986,#6987,#6988)) ;
#1760 = EDGE_LOOP('',(#6989,#6990,#6991,#6992)) ;
#1761 = EDGE_LOOP('',(#6993,#6994,#6995,#6996)) ;
#1762 = EDGE_LOOP('',(#6997,#6998,#6999,#7000)) ;
#1763 = EDGE_LOOP('',(#7001,#7002,#7003,#7004)) ;
#1764 = EDGE_LOOP('',(#7005,#7006,#7007,#7008,#7009,#7010,#7011,#7012)) ;
#1765 = EDGE_LOOP('',(#7013,#7014,#7015,#7016)) ;
#1766 = EDGE_LOOP('',(#7017,#7018,#7019,#7020)) ;
#1767 = EDGE_LOOP('',(#7021,#7022,#7023,#7024)) ;
#1768 = EDGE_LOOP('',(#7025,#7026,#7027,#7028)) ;
#1769 = EDGE_LOOP('',(#7029,#7030,#7031,#7032)) ;
#1770 = EDGE_LOOP('',(#7033,#7034,#7035,#7036)) ;
#1771 = EDGE_LOOP('',(#7037,#7038,#7039,#7040,#7041,#7042,#7043,#7044,#7045,
#7046,#7047,#7048,#7049,#7050,#7051,#7052,#7053,#7054)) ;
#1772 = EDGE_LOOP('',(#7055,#7056,#7057,#7058)) ;
#1773 = EDGE_LOOP('',(#7059,#7060,#7061,#7062)) ;
#1774 = EDGE_LOOP('',(#7063,#7064,#7065,#7066)) ;
#1775 = EDGE_LOOP('',(#7067,#7068,#7069,#7070)) ;
#1776 = EDGE_LOOP('',(#7071,#7072,#7073,#7074)) ;
#1777 = EDGE_LOOP('',(#7075,#7076,#7077,#7078)) ;
#1778 = EDGE_LOOP('',(#7079,#7080,#7081,#7082)) ;
#1779 = EDGE_LOOP('',(#7083,#7084,#7085,#7086)) ;
#1780 = EDGE_LOOP('',(#7087,#7088,#7089,#7090)) ;
#1781 = EDGE_LOOP('',(#7091,#7092,#7093,#7094)) ;
#1782 = EDGE_LOOP('',(#7095,#7096,#7097,#7098)) ;
#1783 = EDGE_LOOP('',(#7099,#7100,#7101,#7102)) ;
#1784 = EDGE_LOOP('',(#7103,#7104,#7105,#7106)) ;
#1785 = EDGE_LOOP('',(#7107)) ;
#1786 = EDGE_LOOP('',(#7108)) ;
#1787 = EDGE_LOOP('',(#7109)) ;
#1788 = EDGE_LOOP('',(#7110)) ;
#1789 = EDGE_LOOP('',(#7111,#7112,#7113,#7114)) ;
#1790 = EDGE_LOOP('',(#7115)) ;
#1791 = EDGE_LOOP('',(#7116)) ;
#1792 = EDGE_LOOP('',(#7117)) ;
#1793 = EDGE_LOOP('',(#7118,#7119,#7120,#7121)) ;
#1794 = EDGE_LOOP('',(#7122,#7123,#7124,#7125)) ;
#1795 = EDGE_LOOP('',(#7126,#7127,#7128,#7129)) ;
#1796 = EDGE_LOOP('',(#7130,#7131,#7132,#7133)) ;
#1797 = EDGE_LOOP('',(#7134,#7135,#7136,#7137)) ;
#1798 = EDGE_LOOP('',(#7138,#7139,#7140,#7141)) ;
#1799 = EDGE_LOOP('',(#7142,#7143,#7144,#7145)) ;
#1800 = EDGE_LOOP('',(#7146,#7147,#7148,#7149)) ;
#1801 = EDGE_LOOP('',(#7150)) ;
#1802 = EDGE_LOOP('',(#7151)) ;
#1803 = EDGE_LOOP('',(#7152)) ;
#1804 = EDGE_LOOP('',(#7153,#7154,#7155,#7156)) ;
#1805 = EDGE_LOOP('',(#7157)) ;
#1806 = EDGE_LOOP('',(#7158)) ;
#1807 = EDGE_LOOP('',(#7159)) ;
#1808 = EDGE_LOOP('',(#7160)) ;
#1809 = EDGE_LOOP('',(#7161,#7162,#7163,#7164)) ;
#1810 = EDGE_LOOP('',(#7165,#7166,#7167,#7168)) ;
#1811 = EDGE_LOOP('',(#7169,#7170,#7171,#7172)) ;
#1812 = EDGE_LOOP('',(#7173,#7174,#7175,#7176)) ;
#1813 = EDGE_LOOP('',(#7177,#7178,#7179,#7180)) ;
#1814 = EDGE_LOOP('',(#7181,#7182,#7183,#7184)) ;
#1815 = EDGE_LOOP('',(#7185,#7186,#7187,#7188)) ;
#1816 = EDGE_LOOP('',(#7189,#7190,#7191,#7192)) ;
#1817 = EDGE_LOOP('',(#7193,#7194,#7195,#7196)) ;
#1818 = EDGE_LOOP('',(#7197,#7198,#7199,#7200)) ;
#1819 = EDGE_LOOP('',(#7201)) ;
#1820 = EDGE_LOOP('',(#7202)) ;
#1821 = EDGE_LOOP('',(#7203)) ;
#1822 = EDGE_LOOP('',(#7204)) ;
#1823 = EDGE_LOOP('',(#7205)) ;
#1824 = EDGE_LOOP('',(#7206,#7207,#7208,#7209)) ;
#1825 = EDGE_LOOP('',(#7210)) ;
#1826 = EDGE_LOOP('',(#7211)) ;
#1827 = EDGE_LOOP('',(#7212)) ;
#1828 = EDGE_LOOP('',(#7213,#7214,#7215,#7216)) ;
#1829 = EDGE_LOOP('',(#7217,#7218,#7219,#7220)) ;
#1830 = EDGE_LOOP('',(#7221,#7222,#7223,#7224)) ;
#1831 = EDGE_LOOP('',(#7225,#7226,#7227,#7228)) ;
#1832 = EDGE_LOOP('',(#7229,#7230,#7231,#7232)) ;
#1833 = EDGE_LOOP('',(#7233,#7234,#7235,#7236)) ;
#1834 = EDGE_LOOP('',(#7237,#7238,#7239,#7240)) ;
#1835 = EDGE_LOOP('',(#7241,#7242,#7243,#7244)) ;
#1836 = EDGE_LOOP('',(#7245)) ;
#1837 = EDGE_LOOP('',(#7246)) ;
#1838 = EDGE_LOOP('',(#7247)) ;
#1839 = EDGE_LOOP('',(#7248,#7249,#7250,#7251)) ;
#1840 = EDGE_LOOP('',(#7252)) ;
#1841 = EDGE_LOOP('',(#7253)) ;
#1842 = EDGE_LOOP('',(#7254)) ;
#1843 = EDGE_LOOP('',(#7255)) ;
#1844 = EDGE_LOOP('',(#7256)) ;
#1845 = EDGE_LOOP('',(#7257,#7258,#7259)) ;
#1846 = EDGE_LOOP('',(#7260,#7261,#7262,#7263,#7264,#7265,#7266)) ;
#1847 = EDGE_LOOP('',(#7267,#7268,#7269,#7270)) ;
#1848 = EDGE_LOOP('',(#7271)) ;
#1849 = EDGE_LOOP('',(#7272,#7273,#7274,#7275)) ;
#1850 = EDGE_LOOP('',(#7276)) ;
#1851 = EDGE_LOOP('',(#7277)) ;
#1852 = EDGE_LOOP('',(#7278,#7279,#7280,#7281)) ;
#1853 = EDGE_LOOP('',(#7282)) ;
#1854 = EDGE_LOOP('',(#7283)) ;
#1855 = EDGE_LOOP('',(#7284,#7285,#7286,#7287)) ;
#1856 = EDGE_LOOP('',(#7288)) ;
#1857 = EDGE_LOOP('',(#7289)) ;
#1858 = EDGE_LOOP('',(#7290,#7291,#7292,#7293,#7294,#7295,#7296,#7297)) ;
#1859 = EDGE_LOOP('',(#7298,#7299,#7300)) ;
#1860 = EDGE_LOOP('',(#7301,#7302)) ;
#1861 = EDGE_LOOP('',(#7303)) ;
#1862 = EDGE_LOOP('',(#7304,#7305)) ;
#1863 = EDGE_LOOP('',(#7306)) ;
#1864 = EDGE_LOOP('',(#7307,#7308,#7309,#7310,#7311,#7312)) ;
#1865 = EDGE_LOOP('',(#7313,#7314,#7315,#7316)) ;
#1866 = EDGE_LOOP('',(#7317,#7318,#7319,#7320,#7321,#7322)) ;
#1867 = EDGE_LOOP('',(#7323,#7324)) ;
#1868 = EDGE_LOOP('',(#7325)) ;
#1869 = EDGE_LOOP('',(#7326,#7327)) ;
#1870 = EDGE_LOOP('',(#7328)) ;
#1871 = EDGE_LOOP('',(#7329,#7330,#7331)) ;
#1872 = EDGE_LOOP('',(#7332,#7333)) ;
#1873 = EDGE_LOOP('',(#7334,#7335,#7336,#7337,#7338,#7339,#7340,#7341,#7342,
#7343)) ;
#1874 = EDGE_LOOP('',(#7344)) ;
#1875 = EDGE_LOOP('',(#7345)) ;
#1876 = EDGE_LOOP('',(#7346,#7347,#7348,#7349)) ;
#1877 = EDGE_LOOP('',(#7350)) ;
#1878 = EDGE_LOOP('',(#7351,#7352,#7353,#7354)) ;
#1879 = EDGE_LOOP('',(#7355,#7356,#7357,#7358,#7359,#7360,#7361,#7362,#7363)) ;
#1880 = EDGE_LOOP('',(#7364,#7365,#7366,#7367)) ;
#1881 = EDGE_LOOP('',(#7368,#7369,#7370,#7371)) ;
#1882 = EDGE_LOOP('',(#7372,#7373,#7374)) ;
#1883 = EDGE_LOOP('',(#7375,#7376,#7377,#7378)) ;
#1884 = EDGE_LOOP('',(#7379,#7380,#7381,#7382,#7383,#7384,#7385)) ;
#1885 = EDGE_LOOP('',(#7386,#7387,#7388,#7389)) ;
#1886 = EDGE_LOOP('',(#7390,#7391,#7392,#7393,#7394,#7395,#7396)) ;
#1887 = EDGE_LOOP('',(#7397,#7398,#7399)) ;
#1888 = EDGE_LOOP('',(#7400,#7401,#7402,#7403,#7404)) ;
#1889 = EDGE_LOOP('',(#7405,#7406)) ;
#1890 = EDGE_LOOP('',(#7407,#7408,#7409,#7410,#7411,#7412,#7413,#7414,#7415,
#7416,#7417,#7418,#7419)) ;
#1891 = EDGE_LOOP('',(#7420,#7421,#7422,#7423,#7424,#7425,#7426)) ;
#1892 = EDGE_LOOP('',(#7427,#7428,#7429,#7430)) ;
#1893 = EDGE_LOOP('',(#7431,#7432,#7433,#7434,#7435,#7436,#7437,#7438)) ;
#1894 = EDGE_LOOP('',(#7439,#7440,#7441,#7442)) ;
#1895 = EDGE_LOOP('',(#7443,#7444,#7445,#7446)) ;
#1896 = EDGE_LOOP('',(#7447,#7448,#7449,#7450)) ;
#1897 = EDGE_LOOP('',(#7451,#7452,#7453,#7454)) ;
#1898 = EDGE_LOOP('',(#7455,#7456,#7457,#7458)) ;
#1899 = EDGE_LOOP('',(#7459,#7460,#7461,#7462)) ;
#1900 = EDGE_LOOP('',(#7463,#7464,#7465,#7466,#7467,#7468,#7469,#7470)) ;
#1901 = EDGE_LOOP('',(#7471,#7472,#7473,#7474)) ;
#1902 = EDGE_LOOP('',(#7475,#7476,#7477,#7478,#7479)) ;
#1903 = EDGE_LOOP('',(#7480)) ;
#1904 = EDGE_LOOP('',(#7481,#7482,#7483,#7484)) ;
#1905 = EDGE_LOOP('',(#7485,#7486,#7487,#7488)) ;
#1906 = EDGE_LOOP('',(#7489,#7490,#7491,#7492)) ;
#1907 = EDGE_LOOP('',(#7493,#7494,#7495,#7496)) ;
#1908 = EDGE_LOOP('',(#7497,#7498,#7499,#7500)) ;
#1909 = EDGE_LOOP('',(#7501,#7502,#7503,#7504,#7505,#7506,#7507,#7508,#7509)) ;
#1910 = EDGE_LOOP('',(#7510)) ;
#1911 = EDGE_LOOP('',(#7511,#7512,#7513,#7514,#7515,#7516)) ;
#1912 = EDGE_LOOP('',(#7517,#7518,#7519,#7520,#7521,#7522)) ;
#1913 = EDGE_LOOP('',(#7523,#7524,#7525,#7526)) ;
#1914 = EDGE_LOOP('',(#7527,#7528,#7529,#7530,#7531,#7532)) ;
#1915 = EDGE_LOOP('',(#7533,#7534,#7535,#7536)) ;
#1916 = EDGE_LOOP('',(#7537,#7538,#7539,#7540)) ;
#1917 = EDGE_LOOP('',(#7541)) ;
#1918 = EDGE_LOOP('',(#7542,#7543,#7544,#7545)) ;
#1919 = EDGE_LOOP('',(#7546,#7547,#7548,#7549)) ;
#1920 = EDGE_LOOP('',(#7550)) ;
#1921 = EDGE_LOOP('',(#7551,#7552,#7553,#7554)) ;
#1922 = EDGE_LOOP('',(#7555,#7556,#7557,#7558,#7559,#7560)) ;
#1923 = EDGE_LOOP('',(#7561,#7562,#7563,#7564,#7565,#7566,#7567,#7568,#7569)) ;
#1924 = EDGE_LOOP('',(#7570,#7571)) ;
#1925 = EDGE_LOOP('',(#7572,#7573,#7574,#7575,#7576,#7577)) ;
#1926 = EDGE_LOOP('',(#7578,#7579,#7580,#7581,#7582,#7583)) ;
#1927 = EDGE_LOOP('',(#7584,#7585,#7586,#7587,#7588,#7589)) ;
#1928 = EDGE_LOOP('',(#7590,#7591,#7592,#7593,#7594,#7595,#7596,#7597,#7598)) ;
#1929 = EDGE_LOOP('',(#7599,#7600)) ;
#1930 = EDGE_LOOP('',(#7601,#7602,#7603,#7604)) ;
#1931 = EDGE_LOOP('',(#7605)) ;
#1932 = EDGE_LOOP('',(#7606)) ;
#1933 = EDGE_LOOP('',(#7607,#7608,#7609,#7610)) ;
#1934 = EDGE_LOOP('',(#7611,#7612,#7613,#7614)) ;
#1935 = EDGE_LOOP('',(#7615,#7616,#7617,#7618)) ;
#1936 = EDGE_LOOP('',(#7619,#7620,#7621,#7622)) ;
#1937 = EDGE_LOOP('',(#7623,#7624,#7625,#7626)) ;
#1938 = EDGE_LOOP('',(#7627,#7628,#7629,#7630)) ;
#1939 = EDGE_LOOP('',(#7631)) ;
#1940 = EDGE_LOOP('',(#7632,#7633,#7634,#7635)) ;
#1941 = EDGE_LOOP('',(#7636)) ;
#1942 = EDGE_LOOP('',(#7637)) ;
#1943 = EDGE_LOOP('',(#7638,#7639,#7640,#7641)) ;
#1944 = EDGE_LOOP('',(#7642,#7643,#7644,#7645)) ;
#1945 = EDGE_LOOP('',(#7646)) ;
#1946 = EDGE_LOOP('',(#7647)) ;
#1947 = EDGE_LOOP('',(#7648,#7649,#7650,#7651)) ;
#1948 = EDGE_LOOP('',(#7652)) ;
#1949 = EDGE_LOOP('',(#7653)) ;
#1950 = EDGE_LOOP('',(#7654,#7655,#7656,#7657)) ;
#1951 = EDGE_LOOP('',(#7658)) ;
#1952 = EDGE_LOOP('',(#7659)) ;
#1953 = EDGE_LOOP('',(#7660,#7661,#7662,#7663)) ;
#1954 = EDGE_LOOP('',(#7664,#7665,#7666,#7667)) ;
#1955 = EDGE_LOOP('',(#7668)) ;
#1956 = EDGE_LOOP('',(#7669,#7670,#7671,#7672)) ;
#1957 = EDGE_LOOP('',(#7673,#7674,#7675,#7676)) ;
#1958 = EDGE_LOOP('',(#7677,#7678,#7679,#7680)) ;
#1959 = EDGE_LOOP('',(#7681,#7682,#7683,#7684)) ;
#1960 = EDGE_LOOP('',(#7685,#7686,#7687,#7688)) ;
#1961 = EDGE_LOOP('',(#7689,#7690,#7691,#7692,#7693,#7694)) ;
#1962 = EDGE_LOOP('',(#7695,#7696,#7697,#7698)) ;
#1963 = EDGE_LOOP('',(#7699,#7700,#7701,#7702,#7703,#7704)) ;
#1964 = EDGE_LOOP('',(#7705)) ;
#1965 = EDGE_LOOP('',(#7706,#7707,#7708,#7709)) ;
#1966 = EDGE_LOOP('',(#7710,#7711,#7712,#7713)) ;
#1967 = EDGE_LOOP('',(#7714,#7715,#7716,#7717)) ;
#1968 = EDGE_LOOP('',(#7718)) ;
#1969 = EDGE_LOOP('',(#7719)) ;
#1970 = EDGE_LOOP('',(#7720,#7721,#7722,#7723)) ;
#1971 = EDGE_LOOP('',(#7724,#7725,#7726,#7727)) ;
#1972 = EDGE_LOOP('',(#7728)) ;
#1973 = EDGE_LOOP('',(#7729,#7730,#7731,#7732)) ;
#1974 = EDGE_LOOP('',(#7733,#7734,#7735,#7736)) ;
#1975 = EDGE_LOOP('',(#7737,#7738,#7739,#7740)) ;
#1976 = EDGE_LOOP('',(#7741,#7742,#7743,#7744)) ;
#1977 = EDGE_LOOP('',(#7745,#7746,#7747,#7748)) ;
#1978 = EDGE_LOOP('',(#7749,#7750,#7751,#7752)) ;
#1979 = EDGE_LOOP('',(#7753,#7754,#7755,#7756)) ;
#1980 = EDGE_LOOP('',(#7757,#7758,#7759,#7760)) ;
#1981 = EDGE_LOOP('',(#7761,#7762,#7763,#7764)) ;
#1982 = EDGE_LOOP('',(#7765,#7766,#7767,#7768)) ;
#1983 = EDGE_LOOP('',(#7769,#7770,#7771,#7772)) ;
#1984 = EDGE_LOOP('',(#7773,#7774,#7775,#7776)) ;
#1985 = EDGE_LOOP('',(#7777,#7778,#7779,#7780)) ;
#1986 = EDGE_LOOP('',(#7781,#7782,#7783,#7784)) ;
#1987 = EDGE_LOOP('',(#7785,#7786,#7787,#7788)) ;
#1988 = EDGE_LOOP('',(#7789,#7790,#7791,#7792)) ;
#1989 = EDGE_LOOP('',(#7793,#7794,#7795,#7796)) ;
#1990 = EDGE_LOOP('',(#7797,#7798,#7799,#7800)) ;
#1991 = EDGE_LOOP('',(#7801,#7802,#7803,#7804)) ;
#1992 = EDGE_LOOP('',(#7805,#7806,#7807,#7808)) ;
#1993 = EDGE_LOOP('',(#7809,#7810,#7811,#7812)) ;
#1994 = EDGE_LOOP('',(#7813,#7814,#7815,#7816)) ;
#1995 = EDGE_LOOP('',(#7817,#7818,#7819,#7820)) ;
#1996 = EDGE_LOOP('',(#7821,#7822,#7823,#7824)) ;
#1997 = EDGE_LOOP('',(#7825,#7826,#7827,#7828)) ;
#1998 = EDGE_LOOP('',(#7829,#7830,#7831,#7832)) ;
#1999 = EDGE_LOOP('',(#7833,#7834,#7835,#7836)) ;
#2000 = EDGE_LOOP('',(#7837,#7838,#7839,#7840)) ;
#2001 = EDGE_LOOP('',(#7841,#7842,#7843,#7844,#7845)) ;
#2002 = EDGE_LOOP('',(#7846,#7847,#7848,#7849,#7850,#7851,#7852,#7853,#7854,
#7855,#7856,#7857,#7858,#7859,#7860,#7861,#7862,#7863,#7864,#7865,#7866,
#7867,#7868,#7869,#7870,#7871,#7872,#7873,#7874,#7875,#7876,#7877)) ;
#2003 = EDGE_LOOP('',(#7878,#7879,#7880,#7881,#7882)) ;
#2004 = EDGE_LOOP('',(#7883,#7884,#7885,#7886)) ;
#2005 = EDGE_LOOP('',(#7887,#7888,#7889,#7890,#7891,#7892,#7893,#7894,#7895,
#7896,#7897,#7898,#7899,#7900,#7901,#7902,#7903,#7904,#7905,#7906,#7907,
#7908,#7909,#7910,#7911,#7912,#7913,#7914,#7915,#7916,#7917,#7918)) ;
#2006 = EDGE_LOOP('',(#7919,#7920,#7921,#7922,#7923,#7924)) ;
#2007 = EDGE_LOOP('',(#7925,#7926,#7927,#7928)) ;
#2008 = EDGE_LOOP('',(#7929)) ;
#2009 = EDGE_LOOP('',(#7930)) ;
#2010 = EDGE_LOOP('',(#7931,#7932,#7933,#7934,#7935,#7936)) ;
#2011 = EDGE_LOOP('',(#7937)) ;
#2012 = EDGE_LOOP('',(#7938,#7939,#7940)) ;
#2013 = EDGE_LOOP('',(#7941,#7942,#7943,#7944)) ;
#2014 = EDGE_LOOP('',(#7945,#7946,#7947,#7948)) ;
#2015 = EDGE_LOOP('',(#7949,#7950,#7951,#7952,#7953,#7954,#7955,#7956,#7957,
#7958,#7959,#7960,#7961,#7962,#7963,#7964,#7965,#7966,#7967,#7968,#7969,
#7970,#7971,#7972,#7973,#7974,#7975,#7976,#7977,#7978,#7979,#7980,#7981,
#7982,#7983,#7984,#7985,#7986,#7987,#7988,#7989,#7990,#7991,#7992,#7993,
#7994,#7995,#7996,#7997,#7998,#7999,#8000,#8001,#8002,#8003,#8004,#8005,
#8006,#8007,#8008,#8009,#8010,#8011,#8012,#8013,#8014,#8015,#8016,#8017,
#8018,#8019,#8020,#8021,#8022,#8023,#8024,#8025,#8026,#8027,#8028,#8029,
#8030,#8031,#8032,#8033,#8034,#8035,#8036,#8037,#8038,#8039,#8040,#8041,
#8042,#8043,#8044,#8045,#8046,#8047,#8048,#8049,#8050,#8051,#8052,#8053,
#8054,#8055,#8056,#8057,#8058,#8059,#8060,#8061,#8062,#8063,#8064,#8065,
#8066,#8067,#8068,#8069,#8070,#8071,#8072,#8073,#8074,#8075,#8076,#8077,
#8078,#8079,#8080,#8081,#8082,#8083,#8084,#8085,#8086,#8087,#8088,#8089,
#8090,#8091,#8092,#8093,#8094,#8095,#8096)) ;
#2016 = EDGE_LOOP('',(#8097,#8098,#8099,#8100)) ;
#2017 = EDGE_LOOP('',(#8101,#8102,#8103,#8104)) ;
#2018 = EDGE_LOOP('',(#8105,#8106,#8107)) ;
#2019 = EDGE_LOOP('',(#8108,#8109,#8110,#8111,#8112,#8113,#8114,#8115,#8116,
#8117,#8118,#8119,#8120,#8121,#8122,#8123,#8124,#8125,#8126,#8127,#8128,
#8129,#8130,#8131,#8132,#8133,#8134,#8135,#8136,#8137,#8138,#8139,#8140,
#8141,#8142,#8143,#8144,#8145,#8146,#8147,#8148,#8149,#8150,#8151,#8152,
#8153,#8154,#8155,#8156,#8157,#8158,#8159,#8160,#8161,#8162,#8163,#8164,
#8165,#8166,#8167,#8168,#8169,#8170,#8171,#8172,#8173,#8174,#8175,#8176,
#8177,#8178,#8179,#8180,#8181,#8182,#8183,#8184,#8185,#8186,#8187,#8188,
#8189,#8190,#8191,#8192,#8193,#8194,#8195,#8196,#8197,#8198,#8199,#8200,
#8201,#8202,#8203,#8204,#8205,#8206,#8207,#8208,#8209,#8210,#8211,#8212,
#8213,#8214,#8215,#8216,#8217,#8218)) ;
#2020 = EDGE_LOOP('',(#8219,#8220,#8221)) ;
#2021 = EDGE_LOOP('',(#8222,#8223,#8224,#8225)) ;
#2022 = EDGE_LOOP('',(#8226,#8227,#8228,#8229)) ;
#2023 = EDGE_LOOP('',(#8230,#8231,#8232,#8233)) ;
#2024 = EDGE_LOOP('',(#8234,#8235,#8236,#8237)) ;
#2025 = EDGE_LOOP('',(#8238,#8239,#8240)) ;
#2026 = EDGE_LOOP('',(#8241,#8242,#8243)) ;
#2027 = EDGE_LOOP('',(#8244,#8245,#8246,#8247)) ;
#2028 = EDGE_LOOP('',(#8248,#8249,#8250,#8251)) ;
#2029 = EDGE_LOOP('',(#8252,#8253,#8254,#8255)) ;
#2030 = EDGE_LOOP('',(#8256,#8257,#8258,#8259)) ;
#2031 = EDGE_LOOP('',(#8260,#8261,#8262)) ;
#2032 = EDGE_LOOP('',(#8263,#8264,#8265)) ;
#2033 = EDGE_LOOP('',(#8266,#8267,#8268,#8269)) ;
#2034 = EDGE_LOOP('',(#8270,#8271,#8272,#8273)) ;
#2035 = EDGE_LOOP('',(#8274,#8275,#8276,#8277)) ;
#2036 = EDGE_LOOP('',(#8278,#8279,#8280,#8281)) ;
#2037 = EDGE_LOOP('',(#8282,#8283,#8284)) ;
#2038 = EDGE_LOOP('',(#8285,#8286,#8287)) ;
#2039 = EDGE_LOOP('',(#8288,#8289,#8290,#8291)) ;
#2040 = EDGE_LOOP('',(#8292,#8293,#8294,#8295)) ;
#2041 = EDGE_LOOP('',(#8296,#8297,#8298,#8299)) ;
#2042 = EDGE_LOOP('',(#8300,#8301,#8302,#8303)) ;
#2043 = EDGE_LOOP('',(#8304,#8305,#8306)) ;
#2044 = EDGE_LOOP('',(#8307,#8308,#8309)) ;
#2045 = EDGE_LOOP('',(#8310,#8311,#8312,#8313)) ;
#2046 = EDGE_LOOP('',(#8314,#8315,#8316,#8317)) ;
#2047 = EDGE_LOOP('',(#8318,#8319,#8320,#8321)) ;
#2048 = EDGE_LOOP('',(#8322,#8323,#8324,#8325)) ;
#2049 = EDGE_LOOP('',(#8326,#8327,#8328)) ;
#2050 = EDGE_LOOP('',(#8329,#8330,#8331)) ;
#2051 = EDGE_LOOP('',(#8332,#8333,#8334,#8335)) ;
#2052 = EDGE_LOOP('',(#8336,#8337,#8338,#8339)) ;
#2053 = EDGE_LOOP('',(#8340,#8341,#8342,#8343)) ;
#2054 = EDGE_LOOP('',(#8344,#8345,#8346,#8347)) ;
#2055 = EDGE_LOOP('',(#8348,#8349,#8350)) ;
#2056 = EDGE_LOOP('',(#8351,#8352,#8353)) ;
#2057 = EDGE_LOOP('',(#8354,#8355,#8356,#8357)) ;
#2058 = EDGE_LOOP('',(#8358,#8359,#8360,#8361)) ;
#2059 = EDGE_LOOP('',(#8362,#8363,#8364,#8365)) ;
#2060 = EDGE_LOOP('',(#8366,#8367,#8368,#8369)) ;
#2061 = EDGE_LOOP('',(#8370,#8371,#8372)) ;
#2062 = EDGE_LOOP('',(#8373,#8374,#8375)) ;
#2063 = EDGE_LOOP('',(#8376,#8377,#8378,#8379)) ;
#2064 = EDGE_LOOP('',(#8380,#8381,#8382,#8383)) ;
#2065 = EDGE_LOOP('',(#8384,#8385,#8386,#8387)) ;
#2066 = EDGE_LOOP('',(#8388,#8389,#8390,#8391)) ;
#2067 = EDGE_LOOP('',(#8392,#8393,#8394,#8395)) ;
#2068 = EDGE_LOOP('',(#8396,#8397,#8398)) ;
#2069 = EDGE_LOOP('',(#8399,#8400,#8401,#8402)) ;
#2070 = EDGE_LOOP('',(#8403,#8404,#8405,#8406)) ;
#2071 = EDGE_LOOP('',(#8407,#8408,#8409,#8410)) ;
#2072 = EDGE_LOOP('',(#8411,#8412,#8413,#8414)) ;
#2073 = EDGE_LOOP('',(#8415,#8416,#8417)) ;
#2074 = EDGE_LOOP('',(#8418,#8419,#8420)) ;
#2075 = EDGE_LOOP('',(#8421,#8422,#8423,#8424)) ;
#2076 = EDGE_LOOP('',(#8425,#8426,#8427,#8428)) ;
#2077 = EDGE_LOOP('',(#8429,#8430,#8431,#8432)) ;
#2078 = EDGE_LOOP('',(#8433,#8434,#8435,#8436)) ;
#2079 = EDGE_LOOP('',(#8437,#8438,#8439)) ;
#2080 = EDGE_LOOP('',(#8440,#8441,#8442)) ;
#2081 = EDGE_LOOP('',(#8443,#8444,#8445,#8446)) ;
#2082 = EDGE_LOOP('',(#8447,#8448,#8449,#8450)) ;
#2083 = EDGE_LOOP('',(#8451,#8452,#8453,#8454)) ;
#2084 = EDGE_LOOP('',(#8455,#8456,#8457,#8458)) ;
#2085 = EDGE_LOOP('',(#8459,#8460,#8461)) ;
#2086 = EDGE_LOOP('',(#8462,#8463,#8464)) ;
#2087 = EDGE_LOOP('',(#8465,#8466,#8467,#8468)) ;
#2088 = EDGE_LOOP('',(#8469,#8470,#8471,#8472)) ;
#2089 = EDGE_LOOP('',(#8473,#8474,#8475,#8476)) ;
#2090 = EDGE_LOOP('',(#8477,#8478,#8479,#8480)) ;
#2091 = EDGE_LOOP('',(#8481,#8482,#8483)) ;
#2092 = EDGE_LOOP('',(#8484,#8485,#8486)) ;
#2093 = EDGE_LOOP('',(#8487,#8488,#8489,#8490)) ;
#2094 = EDGE_LOOP('',(#8491,#8492,#8493,#8494)) ;
#2095 = EDGE_LOOP('',(#8495,#8496,#8497,#8498)) ;
#2096 = EDGE_LOOP('',(#8499,#8500,#8501,#8502)) ;
#2097 = EDGE_LOOP('',(#8503,#8504,#8505)) ;
#2098 = EDGE_LOOP('',(#8506,#8507,#8508)) ;
#2099 = EDGE_LOOP('',(#8509,#8510,#8511,#8512)) ;
#2100 = EDGE_LOOP('',(#8513,#8514,#8515,#8516)) ;
#2101 = EDGE_LOOP('',(#8517,#8518,#8519,#8520)) ;
#2102 = EDGE_LOOP('',(#8521,#8522,#8523,#8524)) ;
#2103 = EDGE_LOOP('',(#8525,#8526,#8527)) ;
#2104 = EDGE_LOOP('',(#8528,#8529,#8530)) ;
#2105 = EDGE_LOOP('',(#8531,#8532,#8533,#8534)) ;
#2106 = EDGE_LOOP('',(#8535,#8536,#8537,#8538)) ;
#2107 = EDGE_LOOP('',(#8539,#8540,#8541,#8542)) ;
#2108 = EDGE_LOOP('',(#8543,#8544,#8545,#8546)) ;
#2109 = EDGE_LOOP('',(#8547,#8548,#8549)) ;
#2110 = EDGE_LOOP('',(#8550,#8551,#8552)) ;
#2111 = EDGE_LOOP('',(#8553,#8554,#8555,#8556)) ;
#2112 = EDGE_LOOP('',(#8557,#8558,#8559,#8560)) ;
#2113 = EDGE_LOOP('',(#8561,#8562,#8563,#8564)) ;
#2114 = EDGE_LOOP('',(#8565,#8566,#8567,#8568)) ;
#2115 = EDGE_LOOP('',(#8569,#8570,#8571)) ;
#2116 = EDGE_LOOP('',(#8572,#8573,#8574)) ;
#2117 = EDGE_LOOP('',(#8575,#8576,#8577,#8578)) ;
#2118 = EDGE_LOOP('',(#8579,#8580,#8581,#8582)) ;
#2119 = EDGE_LOOP('',(#8583,#8584,#8585,#8586)) ;
#2120 = EDGE_LOOP('',(#8587,#8588,#8589,#8590)) ;
#2121 = EDGE_LOOP('',(#8591,#8592,#8593)) ;
#2122 = EDGE_LOOP('',(#8594,#8595,#8596,#8597)) ;
#2123 = EDGE_LOOP('',(#8598)) ;
#2124 = EDGE_LOOP('',(#8599)) ;
#2125 = EDGE_LOOP('',(#8600,#8601,#8602,#8603,#8604,#8605,#8606,#8607,#8608,
#8609,#8610,#8611,#8612,#8613,#8614,#8615,#8616,#8617,#8618,#8619,#8620)) ;
#2126 = EDGE_LOOP('',(#8621,#8622,#8623,#8624)) ;
#2127 = EDGE_LOOP('',(#8625,#8626,#8627,#8628)) ;
#2128 = EDGE_LOOP('',(#8629,#8630,#8631,#8632)) ;
#2129 = EDGE_LOOP('',(#8633,#8634,#8635,#8636)) ;
#2130 = EDGE_LOOP('',(#8637,#8638,#8639,#8640)) ;
#2131 = EDGE_LOOP('',(#8641,#8642,#8643,#8644)) ;
#2132 = EDGE_LOOP('',(#8645,#8646,#8647,#8648,#8649,#8650,#8651,#8652)) ;
#2133 = EDGE_LOOP('',(#8653,#8654,#8655,#8656,#8657,#8658,#8659,#8660)) ;
#2134 = EDGE_LOOP('',(#8661,#8662,#8663,#8664,#8665,#8666,#8667,#8668)) ;
#2135 = EDGE_LOOP('',(#8669,#8670)) ;
#2136 = EDGE_LOOP('',(#8671,#8672)) ;
#2137 = EDGE_LOOP('',(#8673,#8674)) ;
#2138 = EDGE_LOOP('',(#8675,#8676)) ;
#2139 = EDGE_LOOP('',(#8677,#8678)) ;
#2140 = EDGE_LOOP('',(#8679,#8680)) ;
#2141 = EDGE_LOOP('',(#8681,#8682)) ;
#2142 = EDGE_LOOP('',(#8683,#8684)) ;
#2143 = EDGE_LOOP('',(#8685,#8686)) ;
#2144 = EDGE_LOOP('',(#8687,#8688)) ;
#2145 = EDGE_LOOP('',(#8689,#8690)) ;
#2146 = EDGE_LOOP('',(#8691,#8692)) ;
#2147 = EDGE_LOOP('',(#8693,#8694,#8695,#8696,#8697,#8698,#8699,#8700)) ;
#2148 = EDGE_LOOP('',(#8701,#8702,#8703,#8704,#8705,#8706,#8707,#8708)) ;
#2149 = EDGE_LOOP('',(#8709,#8710,#8711,#8712,#8713,#8714,#8715,#8716)) ;
#2150 = EDGE_LOOP('',(#8717,#8718,#8719,#8720,#8721,#8722,#8723,#8724)) ;
#2151 = EDGE_LOOP('',(#8725,#8726,#8727,#8728)) ;
#2152 = EDGE_LOOP('',(#8729,#8730,#8731,#8732)) ;
#2153 = EDGE_LOOP('',(#8733,#8734,#8735,#8736,#8737,#8738)) ;
#2154 = EDGE_LOOP('',(#8739,#8740,#8741,#8742)) ;
#2155 = EDGE_LOOP('',(#8743,#8744,#8745,#8746)) ;
#2156 = EDGE_LOOP('',(#8747,#8748,#8749,#8750)) ;
#2157 = EDGE_LOOP('',(#8751,#8752,#8753,#8754)) ;
#2158 = EDGE_LOOP('',(#8755,#8756,#8757,#8758,#8759,#8760,#8761,#8762)) ;
#2159 = EDGE_LOOP('',(#8763)) ;
#2160 = EDGE_LOOP('',(#8764,#8765,#8766,#8767)) ;
#2161 = EDGE_LOOP('',(#8768)) ;
#2162 = EDGE_LOOP('',(#8769,#8770,#8771,#8772,#8773)) ;
#2163 = EDGE_LOOP('',(#8774,#8775,#8776,#8777,#8778,#8779,#8780,#8781)) ;
#2164 = EDGE_LOOP('',(#8782)) ;
#2165 = EDGE_LOOP('',(#8783,#8784,#8785,#8786)) ;
#2166 = EDGE_LOOP('',(#8787,#8788,#8789,#8790)) ;
#2167 = EDGE_LOOP('',(#8791,#8792,#8793,#8794)) ;
#2168 = EDGE_LOOP('',(#8795,#8796,#8797,#8798)) ;
#2169 = EDGE_LOOP('',(#8799,#8800,#8801,#8802,#8803,#8804)) ;
#2170 = EDGE_LOOP('',(#8805,#8806,#8807,#8808)) ;
#2171 = EDGE_LOOP('',(#8809)) ;
#2172 = EDGE_LOOP('',(#8810,#8811,#8812,#8813,#8814,#8815,#8816,#8817,#8818,
#8819,#8820,#8821)) ;
#2173 = EDGE_LOOP('',(#8822)) ;
#2174 = EDGE_LOOP('',(#8823,#8824,#8825,#8826)) ;
#2175 = EDGE_LOOP('',(#8827,#8828,#8829,#8830)) ;
#2176 = EDGE_LOOP('',(#8831,#8832,#8833,#8834)) ;
#2177 = EDGE_LOOP('',(#8835,#8836,#8837,#8838)) ;
#2178 = EDGE_LOOP('',(#8839,#8840,#8841,#8842)) ;
#2179 = EDGE_LOOP('',(#8843,#8844,#8845,#8846)) ;
#2180 = EDGE_LOOP('',(#8847)) ;
#2181 = EDGE_LOOP('',(#8848)) ;
#2182 = EDGE_LOOP('',(#8849)) ;
#2183 = EDGE_LOOP('',(#8850,#8851,#8852,#8853)) ;
#2184 = EDGE_LOOP('',(#8854)) ;
#2185 = EDGE_LOOP('',(#8855)) ;
#2186 = EDGE_LOOP('',(#8856)) ;
#2187 = EDGE_LOOP('',(#8857,#8858,#8859,#8860)) ;
#2188 = EDGE_LOOP('',(#8861,#8862,#8863,#8864)) ;
#2189 = EDGE_LOOP('',(#8865,#8866,#8867,#8868)) ;
#2190 = EDGE_LOOP('',(#8869)) ;
#2191 = EDGE_LOOP('',(#8870,#8871,#8872,#8873)) ;
#2192 = EDGE_LOOP('',(#8874,#8875,#8876,#8877)) ;
#2193 = EDGE_LOOP('',(#8878,#8879,#8880,#8881)) ;
#2194 = EDGE_LOOP('',(#8882,#8883,#8884,#8885)) ;
#2195 = EDGE_LOOP('',(#8886,#8887,#8888,#8889)) ;
#2196 = EDGE_LOOP('',(#8890)) ;
#2197 = EDGE_LOOP('',(#8891,#8892,#8893,#8894)) ;
#2198 = EDGE_LOOP('',(#8895)) ;
#2199 = EDGE_LOOP('',(#8896,#8897,#8898,#8899)) ;
#2200 = EDGE_LOOP('',(#8900,#8901,#8902,#8903)) ;
#2201 = EDGE_LOOP('',(#8904,#8905,#8906,#8907)) ;
#2202 = EDGE_LOOP('',(#8908,#8909,#8910,#8911)) ;
#2203 = EDGE_LOOP('',(#8912,#8913,#8914,#8915)) ;
#2204 = EDGE_LOOP('',(#8916)) ;
#2205 = EDGE_LOOP('',(#8917,#8918,#8919,#8920)) ;
#2206 = EDGE_LOOP('',(#8921,#8922,#8923,#8924)) ;
#2207 = EDGE_LOOP('',(#8925,#8926,#8927,#8928)) ;
#2208 = EDGE_LOOP('',(#8929,#8930,#8931,#8932)) ;
#2209 = EDGE_LOOP('',(#8933,#8934,#8935,#8936)) ;
#2210 = EDGE_LOOP('',(#8937)) ;
#2211 = EDGE_LOOP('',(#8938)) ;
#2212 = EDGE_LOOP('',(#8939,#8940,#8941,#8942)) ;
#2213 = EDGE_LOOP('',(#8943)) ;
#2214 = EDGE_LOOP('',(#8944)) ;
#2215 = EDGE_LOOP('',(#8945,#8946,#8947,#8948)) ;
#2216 = EDGE_LOOP('',(#8949,#8950,#8951,#8952)) ;
#2217 = EDGE_LOOP('',(#8953)) ;
#2218 = EDGE_LOOP('',(#8954)) ;
#2219 = EDGE_LOOP('',(#8955,#8956,#8957,#8958)) ;
#2220 = EDGE_LOOP('',(#8959)) ;
#2221 = EDGE_LOOP('',(#8960)) ;
#2222 = EDGE_LOOP('',(#8961,#8962,#8963,#8964)) ;
#2223 = EDGE_LOOP('',(#8965,#8966,#8967,#8968)) ;
#2224 = EDGE_LOOP('',(#8969,#8970,#8971,#8972)) ;
#2225 = EDGE_LOOP('',(#8973,#8974,#8975,#8976)) ;
#2226 = EDGE_LOOP('',(#8977,#8978,#8979,#8980)) ;
#2227 = EDGE_LOOP('',(#8981)) ;
#2228 = EDGE_LOOP('',(#8982)) ;
#2229 = EDGE_LOOP('',(#8983,#8984,#8985,#8986)) ;
#2230 = EDGE_LOOP('',(#8987)) ;
#2231 = EDGE_LOOP('',(#8988)) ;
#2232 = EDGE_LOOP('',(#8989,#8990,#8991,#8992)) ;
#2233 = LINE('',#13428,#3004) ;
#2234 = LINE('',#13433,#3005) ;
#2235 = LINE('',#13435,#3006) ;
#2236 = LINE('',#13437,#3007) ;
#2237 = LINE('',#13438,#3008) ;
#2238 = LINE('',#13443,#3009) ;
#2239 = LINE('',#13449,#3010) ;
#2240 = LINE('',#13454,#3011) ;
#2241 = LINE('',#13456,#3012) ;
#2242 = LINE('',#13458,#3013) ;
#2243 = LINE('',#13459,#3014) ;
#2244 = LINE('',#13464,#3015) ;
#2245 = LINE('',#13470,#3016) ;
#2246 = LINE('',#13475,#3017) ;
#2247 = LINE('',#13477,#3018) ;
#2248 = LINE('',#13479,#3019) ;
#2249 = LINE('',#13480,#3020) ;
#2250 = LINE('',#13485,#3021) ;
#2251 = LINE('',#13491,#3022) ;
#2252 = LINE('',#13496,#3023) ;
#2253 = LINE('',#13498,#3024) ;
#2254 = LINE('',#13500,#3025) ;
#2255 = LINE('',#13501,#3026) ;
#2256 = LINE('',#13506,#3027) ;
#2257 = LINE('',#13510,#3028) ;
#2258 = LINE('',#13514,#3029) ;
#2259 = LINE('',#13556,#3030) ;
#2260 = LINE('',#13560,#3031) ;
#2261 = LINE('',#13602,#3032) ;
#2262 = LINE('',#13606,#3033) ;
#2263 = LINE('',#13610,#3034) ;
#2264 = LINE('',#13614,#3035) ;
#2265 = LINE('',#13618,#3036) ;
#2266 = LINE('',#13621,#3037) ;
#2267 = LINE('',#13624,#3038) ;
#2268 = LINE('',#13627,#3039) ;
#2269 = LINE('',#13640,#3040) ;
#2270 = LINE('',#13644,#3041) ;
#2271 = LINE('',#13657,#3042) ;
#2272 = LINE('',#13661,#3043) ;
#2273 = LINE('',#13702,#3044) ;
#2274 = LINE('',#13744,#3045) ;
#2275 = LINE('',#13787,#3046) ;
#2276 = LINE('',#13829,#3047) ;
#2277 = LINE('',#13836,#3048) ;
#2278 = LINE('',#13842,#3049) ;
#2279 = LINE('',#13847,#3050) ;
#2280 = LINE('',#13851,#3051) ;
#2281 = LINE('',#13856,#3052) ;
#2282 = LINE('',#13860,#3053) ;
#2283 = LINE('',#13864,#3054) ;
#2284 = LINE('',#13866,#3055) ;
#2285 = LINE('',#13867,#3056) ;
#2286 = LINE('',#13872,#3057) ;
#2287 = LINE('',#13874,#3058) ;
#2288 = LINE('',#13875,#3059) ;
#2289 = LINE('',#13878,#3060) ;
#2290 = LINE('',#13880,#3061) ;
#2291 = LINE('',#13881,#3062) ;
#2292 = LINE('',#13886,#3063) ;
#2293 = LINE('',#13888,#3064) ;
#2294 = LINE('',#13889,#3065) ;
#2295 = LINE('',#13893,#3066) ;
#2296 = LINE('',#13895,#3067) ;
#2297 = LINE('',#13897,#3068) ;
#2298 = LINE('',#13898,#3069) ;
#2299 = LINE('',#13901,#3070) ;
#2300 = LINE('',#13903,#3071) ;
#2301 = LINE('',#13905,#3072) ;
#2302 = LINE('',#13907,#3073) ;
#2303 = LINE('',#13908,#3074) ;
#2304 = LINE('',#13911,#3075) ;
#2305 = LINE('',#13913,#3076) ;
#2306 = LINE('',#13915,#3077) ;
#2307 = LINE('',#13917,#3078) ;
#2308 = LINE('',#13919,#3079) ;
#2309 = LINE('',#13921,#3080) ;
#2310 = LINE('',#13923,#3081) ;
#2311 = LINE('',#13925,#3082) ;
#2312 = LINE('',#13927,#3083) ;
#2313 = LINE('',#13929,#3084) ;
#2314 = LINE('',#13931,#3085) ;
#2315 = LINE('',#13933,#3086) ;
#2316 = LINE('',#13934,#3087) ;
#2317 = LINE('',#13936,#3088) ;
#2318 = LINE('',#13938,#3089) ;
#2319 = LINE('',#13939,#3090) ;
#2320 = LINE('',#13941,#3091) ;
#2321 = LINE('',#13942,#3092) ;
#2322 = LINE('',#13945,#3093) ;
#2323 = LINE('',#13947,#3094) ;
#2324 = LINE('',#13948,#3095) ;
#2325 = LINE('',#13951,#3096) ;
#2326 = LINE('',#13953,#3097) ;
#2327 = LINE('',#13955,#3098) ;
#2328 = LINE('',#13956,#3099) ;
#2329 = LINE('',#13961,#3100) ;
#2330 = LINE('',#13965,#3101) ;
#2331 = LINE('',#13971,#3102) ;
#2332 = LINE('',#13975,#3103) ;
#2333 = LINE('',#13979,#3104) ;
#2334 = LINE('',#13981,#3105) ;
#2335 = LINE('',#13983,#3106) ;
#2336 = LINE('',#13985,#3107) ;
#2337 = LINE('',#13987,#3108) ;
#2338 = LINE('',#13989,#3109) ;
#2339 = LINE('',#13991,#3110) ;
#2340 = LINE('',#13993,#3111) ;
#2341 = LINE('',#13995,#3112) ;
#2342 = LINE('',#13997,#3113) ;
#2343 = LINE('',#13998,#3114) ;
#2344 = LINE('',#14000,#3115) ;
#2345 = LINE('',#14002,#3116) ;
#2346 = LINE('',#14003,#3117) ;
#2347 = LINE('',#14005,#3118) ;
#2348 = LINE('',#14007,#3119) ;
#2349 = LINE('',#14008,#3120) ;
#2350 = LINE('',#14012,#3121) ;
#2351 = LINE('',#14015,#3122) ;
#2352 = LINE('',#14016,#3123) ;
#2353 = LINE('',#14023,#3124) ;
#2354 = LINE('',#14025,#3125) ;
#2355 = LINE('',#14027,#3126) ;
#2356 = LINE('',#14028,#3127) ;
#2357 = LINE('',#14031,#3128) ;
#2358 = LINE('',#14033,#3129) ;
#2359 = LINE('',#14034,#3130) ;
#2360 = LINE('',#14037,#3131) ;
#2361 = LINE('',#14038,#3132) ;
#2362 = LINE('',#14043,#3133) ;
#2363 = LINE('',#14052,#3134) ;
#2364 = LINE('',#14055,#3135) ;
#2365 = LINE('',#14056,#3136) ;
#2366 = LINE('',#14063,#3137) ;
#2367 = LINE('',#14065,#3138) ;
#2368 = LINE('',#14067,#3139) ;
#2369 = LINE('',#14068,#3140) ;
#2370 = LINE('',#14071,#3141) ;
#2371 = LINE('',#14073,#3142) ;
#2372 = LINE('',#14074,#3143) ;
#2373 = LINE('',#14077,#3144) ;
#2374 = LINE('',#14078,#3145) ;
#2375 = LINE('',#14081,#3146) ;
#2376 = LINE('',#14083,#3147) ;
#2377 = LINE('',#14084,#3148) ;
#2378 = LINE('',#14087,#3149) ;
#2379 = LINE('',#14089,#3150) ;
#2380 = LINE('',#14090,#3151) ;
#2381 = LINE('',#14092,#3152) ;
#2382 = LINE('',#14093,#3153) ;
#2383 = LINE('',#14095,#3154) ;
#2384 = LINE('',#14098,#3155) ;
#2385 = LINE('',#14100,#3156) ;
#2386 = LINE('',#14101,#3157) ;
#2387 = LINE('',#14103,#3158) ;
#2388 = LINE('',#14104,#3159) ;
#2389 = LINE('',#14107,#3160) ;
#2390 = LINE('',#14108,#3161) ;
#2391 = LINE('',#14111,#3162) ;
#2392 = LINE('',#14112,#3163) ;
#2393 = LINE('',#14114,#3164) ;
#2394 = LINE('',#14116,#3165) ;
#2395 = LINE('',#14117,#3166) ;
#2396 = LINE('',#14118,#3167) ;
#2397 = LINE('',#14120,#3168) ;
#2398 = LINE('',#14121,#3169) ;
#2399 = LINE('',#14124,#3170) ;
#2400 = LINE('',#14126,#3171) ;
#2401 = LINE('',#14127,#3172) ;
#2402 = LINE('',#14129,#3173) ;
#2403 = LINE('',#14130,#3174) ;
#2404 = LINE('',#14133,#3175) ;
#2405 = LINE('',#14134,#3176) ;
#2406 = LINE('',#14137,#3177) ;
#2407 = LINE('',#14138,#3178) ;
#2408 = LINE('',#14139,#3179) ;
#2409 = LINE('',#14141,#3180) ;
#2410 = LINE('',#14143,#3181) ;
#2411 = LINE('',#14145,#3182) ;
#2412 = LINE('',#14147,#3183) ;
#2413 = LINE('',#14150,#3184) ;
#2414 = LINE('',#14151,#3185) ;
#2415 = LINE('',#14154,#3186) ;
#2416 = LINE('',#14155,#3187) ;
#2417 = LINE('',#14157,#3188) ;
#2418 = LINE('',#14159,#3189) ;
#2419 = LINE('',#14162,#3190) ;
#2420 = LINE('',#14164,#3191) ;
#2421 = LINE('',#14171,#3192) ;
#2422 = LINE('',#14177,#3193) ;
#2423 = LINE('',#14182,#3194) ;
#2424 = LINE('',#14184,#3195) ;
#2425 = LINE('',#14186,#3196) ;
#2426 = LINE('',#14187,#3197) ;
#2427 = LINE('',#14190,#3198) ;
#2428 = LINE('',#14192,#3199) ;
#2429 = LINE('',#14194,#3200) ;
#2430 = LINE('',#14196,#3201) ;
#2431 = LINE('',#14197,#3202) ;
#2432 = LINE('',#14200,#3203) ;
#2433 = LINE('',#14202,#3204) ;
#2434 = LINE('',#14203,#3205) ;
#2435 = LINE('',#14205,#3206) ;
#2436 = LINE('',#14208,#3207) ;
#2437 = LINE('',#14210,#3208) ;
#2438 = LINE('',#14211,#3209) ;
#2439 = LINE('',#14216,#3210) ;
#2440 = LINE('',#14222,#3211) ;
#2441 = LINE('',#14229,#3212) ;
#2442 = LINE('',#14233,#3213) ;
#2443 = LINE('',#14237,#3214) ;
#2444 = LINE('',#14240,#3215) ;
#2445 = LINE('',#14242,#3216) ;
#2446 = LINE('',#14246,#3217) ;
#2447 = LINE('',#14248,#3218) ;
#2448 = LINE('',#14252,#3219) ;
#2449 = LINE('',#14256,#3220) ;
#2450 = LINE('',#14259,#3221) ;
#2451 = LINE('',#14263,#3222) ;
#2452 = LINE('',#14265,#3223) ;
#2453 = LINE('',#14267,#3224) ;
#2454 = LINE('',#14268,#3225) ;
#2455 = LINE('',#14271,#3226) ;
#2456 = LINE('',#14273,#3227) ;
#2457 = LINE('',#14274,#3228) ;
#2458 = LINE('',#14277,#3229) ;
#2459 = LINE('',#14278,#3230) ;
#2460 = LINE('',#14280,#3231) ;
#2461 = LINE('',#14281,#3232) ;
#2462 = LINE('',#14283,#3233) ;
#2463 = LINE('',#14286,#3234) ;
#2464 = LINE('',#14287,#3235) ;
#2465 = LINE('',#14291,#3236) ;
#2466 = LINE('',#14294,#3237) ;
#2467 = LINE('',#14301,#3238) ;
#2468 = LINE('',#14304,#3239) ;
#2469 = LINE('',#14315,#3240) ;
#2470 = LINE('',#14316,#3241) ;
#2471 = LINE('',#14327,#3242) ;
#2472 = LINE('',#14328,#3243) ;
#2473 = LINE('',#14339,#3244) ;
#2474 = LINE('',#14340,#3245) ;
#2475 = LINE('',#14345,#3246) ;
#2476 = LINE('',#14346,#3247) ;
#2477 = LINE('',#14348,#3248) ;
#2478 = LINE('',#14350,#3249) ;
#2479 = LINE('',#14352,#3250) ;
#2480 = LINE('',#14356,#3251) ;
#2481 = LINE('',#14358,#3252) ;
#2482 = LINE('',#14359,#3253) ;
#2483 = LINE('',#14362,#3254) ;
#2484 = LINE('',#14365,#3255) ;
#2485 = LINE('',#14367,#3256) ;
#2486 = LINE('',#14370,#3257) ;
#2487 = LINE('',#14371,#3258) ;
#2488 = LINE('',#14376,#3259) ;
#2489 = LINE('',#14378,#3260) ;
#2490 = LINE('',#14380,#3261) ;
#2491 = LINE('',#14387,#3262) ;
#2492 = LINE('',#14393,#3263) ;
#2493 = LINE('',#14399,#3264) ;
#2494 = LINE('',#14405,#3265) ;
#2495 = LINE('',#14410,#3266) ;
#2496 = LINE('',#14412,#3267) ;
#2497 = LINE('',#14414,#3268) ;
#2498 = LINE('',#14415,#3269) ;
#2499 = LINE('',#14421,#3270) ;
#2500 = LINE('',#14424,#3271) ;
#2501 = LINE('',#14426,#3272) ;
#2502 = LINE('',#14427,#3273) ;
#2503 = LINE('',#14437,#3274) ;
#2504 = LINE('',#14443,#3275) ;
#2505 = LINE('',#14449,#3276) ;
#2506 = LINE('',#14454,#3277) ;
#2507 = LINE('',#14456,#3278) ;
#2508 = LINE('',#14458,#3279) ;
#2509 = LINE('',#14459,#3280) ;
#2510 = LINE('',#14465,#3281) ;
#2511 = LINE('',#14468,#3282) ;
#2512 = LINE('',#14470,#3283) ;
#2513 = LINE('',#14471,#3284) ;
#2514 = LINE('',#14482,#3285) ;
#2515 = LINE('',#14488,#3286) ;
#2516 = LINE('',#14494,#3287) ;
#2517 = LINE('',#14500,#3288) ;
#2518 = LINE('',#14506,#3289) ;
#2519 = LINE('',#14511,#3290) ;
#2520 = LINE('',#14513,#3291) ;
#2521 = LINE('',#14515,#3292) ;
#2522 = LINE('',#14516,#3293) ;
#2523 = LINE('',#14522,#3294) ;
#2524 = LINE('',#14525,#3295) ;
#2525 = LINE('',#14527,#3296) ;
#2526 = LINE('',#14528,#3297) ;
#2527 = LINE('',#14538,#3298) ;
#2528 = LINE('',#14544,#3299) ;
#2529 = LINE('',#14550,#3300) ;
#2530 = LINE('',#14555,#3301) ;
#2531 = LINE('',#14557,#3302) ;
#2532 = LINE('',#14559,#3303) ;
#2533 = LINE('',#14560,#3304) ;
#2534 = LINE('',#14566,#3305) ;
#2535 = LINE('',#14569,#3306) ;
#2536 = LINE('',#14571,#3307) ;
#2537 = LINE('',#14572,#3308) ;
#2538 = LINE('',#14582,#3309) ;
#2539 = LINE('',#14592,#3310) ;
#2540 = LINE('',#14640,#3311) ;
#2541 = LINE('',#14647,#3312) ;
#2542 = LINE('',#14654,#3313) ;
#2543 = LINE('',#14662,#3314) ;
#2544 = LINE('',#14671,#3315) ;
#2545 = LINE('',#14680,#3316) ;
#2546 = LINE('',#14693,#3317) ;
#2547 = LINE('',#14708,#3318) ;
#2548 = LINE('',#14722,#3319) ;
#2549 = LINE('',#14743,#3320) ;
#2550 = LINE('',#14750,#3321) ;
#2551 = LINE('',#14756,#3322) ;
#2552 = LINE('',#14760,#3323) ;
#2553 = LINE('',#14764,#3324) ;
#2554 = LINE('',#14766,#3325) ;
#2555 = LINE('',#14768,#3326) ;
#2556 = LINE('',#14770,#3327) ;
#2557 = LINE('',#14776,#3328) ;
#2558 = LINE('',#14778,#3329) ;
#2559 = LINE('',#14779,#3330) ;
#2560 = LINE('',#14782,#3331) ;
#2561 = LINE('',#14783,#3332) ;
#2562 = LINE('',#14786,#3333) ;
#2563 = LINE('',#14787,#3334) ;
#2564 = LINE('',#14793,#3335) ;
#2565 = LINE('',#14794,#3336) ;
#2566 = LINE('',#14797,#3337) ;
#2567 = LINE('',#14800,#3338) ;
#2568 = LINE('',#14802,#3339) ;
#2569 = LINE('',#14803,#3340) ;
#2570 = LINE('',#14805,#3341) ;
#2571 = LINE('',#14810,#3342) ;
#2572 = LINE('',#14821,#3343) ;
#2573 = LINE('',#14825,#3344) ;
#2574 = LINE('',#14828,#3345) ;
#2575 = LINE('',#14830,#3346) ;
#2576 = LINE('',#14834,#3347) ;
#2577 = LINE('',#14836,#3348) ;
#2578 = LINE('',#14838,#3349) ;
#2579 = LINE('',#14840,#3350) ;
#2580 = LINE('',#14841,#3351) ;
#2581 = LINE('',#14845,#3352) ;
#2582 = LINE('',#14846,#3353) ;
#2583 = LINE('',#14847,#3354) ;
#2584 = LINE('',#14850,#3355) ;
#2585 = LINE('',#14851,#3356) ;
#2586 = LINE('',#14854,#3357) ;
#2587 = LINE('',#14855,#3358) ;
#2588 = LINE('',#14857,#3359) ;
#2589 = LINE('',#14863,#3360) ;
#2590 = LINE('',#14865,#3361) ;
#2591 = LINE('',#14867,#3362) ;
#2592 = LINE('',#14868,#3363) ;
#2593 = LINE('',#14871,#3364) ;
#2594 = LINE('',#14873,#3365) ;
#2595 = LINE('',#14874,#3366) ;
#2596 = LINE('',#14877,#3367) ;
#2597 = LINE('',#14879,#3368) ;
#2598 = LINE('',#14880,#3369) ;
#2599 = LINE('',#14884,#3370) ;
#2600 = LINE('',#14885,#3371) ;
#2601 = LINE('',#14887,#3372) ;
#2602 = LINE('',#14889,#3373) ;
#2603 = LINE('',#14890,#3374) ;
#2604 = LINE('',#14892,#3375) ;
#2605 = LINE('',#14895,#3376) ;
#2606 = LINE('',#14899,#3377) ;
#2607 = LINE('',#14905,#3378) ;
#2608 = LINE('',#14906,#3379) ;
#2609 = LINE('',#14909,#3380) ;
#2610 = LINE('',#14913,#3381) ;
#2611 = LINE('',#14917,#3382) ;
#2612 = LINE('',#14918,#3383) ;
#2613 = LINE('',#14964,#3384) ;
#2614 = LINE('',#15025,#3385) ;
#2615 = LINE('',#15087,#3386) ;
#2616 = LINE('',#15094,#3387) ;
#2617 = LINE('',#15096,#3388) ;
#2618 = LINE('',#15098,#3389) ;
#2619 = LINE('',#15100,#3390) ;
#2620 = LINE('',#15101,#3391) ;
#2621 = LINE('',#15104,#3392) ;
#2622 = LINE('',#15106,#3393) ;
#2623 = LINE('',#15107,#3394) ;
#2624 = LINE('',#15111,#3395) ;
#2625 = LINE('',#15112,#3396) ;
#2626 = LINE('',#15113,#3397) ;
#2627 = LINE('',#15116,#3398) ;
#2628 = LINE('',#15117,#3399) ;
#2629 = LINE('',#15119,#3400) ;
#2630 = LINE('',#15122,#3401) ;
#2631 = LINE('',#15123,#3402) ;
#2632 = LINE('',#15129,#3403) ;
#2633 = LINE('',#15131,#3404) ;
#2634 = LINE('',#15143,#3405) ;
#2635 = LINE('',#15154,#3406) ;
#2636 = LINE('',#15156,#3407) ;
#2637 = LINE('',#15165,#3408) ;
#2638 = LINE('',#15170,#3409) ;
#2639 = LINE('',#15172,#3410) ;
#2640 = LINE('',#15174,#3411) ;
#2641 = LINE('',#15175,#3412) ;
#2642 = LINE('',#15181,#3413) ;
#2643 = LINE('',#15184,#3414) ;
#2644 = LINE('',#15186,#3415) ;
#2645 = LINE('',#15187,#3416) ;
#2646 = LINE('',#15200,#3417) ;
#2647 = LINE('',#15204,#3418) ;
#2648 = LINE('',#15211,#3419) ;
#2649 = LINE('',#15218,#3420) ;
#2650 = LINE('',#15225,#3421) ;
#2651 = LINE('',#15229,#3422) ;
#2652 = LINE('',#15235,#3423) ;
#2653 = LINE('',#15237,#3424) ;
#2654 = LINE('',#15239,#3425) ;
#2655 = LINE('',#15240,#3426) ;
#2656 = LINE('',#15244,#3427) ;
#2657 = LINE('',#15246,#3428) ;
#2658 = LINE('',#15248,#3429) ;
#2659 = LINE('',#15249,#3430) ;
#2660 = LINE('',#15252,#3431) ;
#2661 = LINE('',#15254,#3432) ;
#2662 = LINE('',#15255,#3433) ;
#2663 = LINE('',#15258,#3434) ;
#2664 = LINE('',#15260,#3435) ;
#2665 = LINE('',#15261,#3436) ;
#2666 = LINE('',#15277,#3437) ;
#2667 = LINE('',#15281,#3438) ;
#2668 = LINE('',#15285,#3439) ;
#2669 = LINE('',#15292,#3440) ;
#2670 = LINE('',#15296,#3441) ;
#2671 = LINE('',#15302,#3442) ;
#2672 = LINE('',#15326,#3443) ;
#2673 = LINE('',#15374,#3444) ;
#2674 = LINE('',#15422,#3445) ;
#2675 = LINE('',#15476,#3446) ;
#2676 = LINE('',#15524,#3447) ;
#2677 = LINE('',#15572,#3448) ;
#2678 = LINE('',#15626,#3449) ;
#2679 = LINE('',#15674,#3450) ;
#2680 = LINE('',#15722,#3451) ;
#2681 = LINE('',#15776,#3452) ;
#2682 = LINE('',#15824,#3453) ;
#2683 = LINE('',#15872,#3454) ;
#2684 = LINE('',#15926,#3455) ;
#2685 = LINE('',#15974,#3456) ;
#2686 = LINE('',#15990,#3457) ;
#2687 = LINE('',#16014,#3458) ;
#2688 = LINE('',#16039,#3459) ;
#2689 = LINE('',#16064,#3460) ;
#2690 = LINE('',#16088,#3461) ;
#2691 = LINE('',#16113,#3462) ;
#2692 = LINE('',#16138,#3463) ;
#2693 = LINE('',#16162,#3464) ;
#2694 = LINE('',#16187,#3465) ;
#2695 = LINE('',#16212,#3466) ;
#2696 = LINE('',#16236,#3467) ;
#2697 = LINE('',#16261,#3468) ;
#2698 = LINE('',#16286,#3469) ;
#2699 = LINE('',#17420,#3470) ;
#2700 = LINE('',#17428,#3471) ;
#2701 = LINE('',#17429,#3472) ;
#2702 = LINE('',#17432,#3473) ;
#2703 = LINE('',#17434,#3474) ;
#2704 = LINE('',#17440,#3475) ;
#2705 = LINE('',#17448,#3476) ;
#2706 = LINE('',#17452,#3477) ;
#2707 = LINE('',#17456,#3478) ;
#2708 = LINE('',#17460,#3479) ;
#2709 = LINE('',#17464,#3480) ;
#2710 = LINE('',#17468,#3481) ;
#2711 = LINE('',#17472,#3482) ;
#2712 = LINE('',#17476,#3483) ;
#2713 = LINE('',#17480,#3484) ;
#2714 = LINE('',#17484,#3485) ;
#2715 = LINE('',#17488,#3486) ;
#2716 = LINE('',#17492,#3487) ;
#2717 = LINE('',#17496,#3488) ;
#2718 = LINE('',#17500,#3489) ;
#2719 = LINE('',#17504,#3490) ;
#2720 = LINE('',#17508,#3491) ;
#2721 = LINE('',#17512,#3492) ;
#2722 = LINE('',#17516,#3493) ;
#2723 = LINE('',#17520,#3494) ;
#2724 = LINE('',#17524,#3495) ;
#2725 = LINE('',#17528,#3496) ;
#2726 = LINE('',#17532,#3497) ;
#2727 = LINE('',#17536,#3498) ;
#2728 = LINE('',#17540,#3499) ;
#2729 = LINE('',#17544,#3500) ;
#2730 = LINE('',#17548,#3501) ;
#2731 = LINE('',#17552,#3502) ;
#2732 = LINE('',#17556,#3503) ;
#2733 = LINE('',#17560,#3504) ;
#2734 = LINE('',#17564,#3505) ;
#2735 = LINE('',#17568,#3506) ;
#2736 = LINE('',#17572,#3507) ;
#2737 = LINE('',#17576,#3508) ;
#2738 = LINE('',#17580,#3509) ;
#2739 = LINE('',#17584,#3510) ;
#2740 = LINE('',#17588,#3511) ;
#2741 = LINE('',#17592,#3512) ;
#2742 = LINE('',#17596,#3513) ;
#2743 = LINE('',#17601,#3514) ;
#2744 = LINE('',#17605,#3515) ;
#2745 = LINE('',#17609,#3516) ;
#2746 = LINE('',#17613,#3517) ;
#2747 = LINE('',#17617,#3518) ;
#2748 = LINE('',#17621,#3519) ;
#2749 = LINE('',#17625,#3520) ;
#2750 = LINE('',#17629,#3521) ;
#2751 = LINE('',#17633,#3522) ;
#2752 = LINE('',#17637,#3523) ;
#2753 = LINE('',#17641,#3524) ;
#2754 = LINE('',#17645,#3525) ;
#2755 = LINE('',#17649,#3526) ;
#2756 = LINE('',#17653,#3527) ;
#2757 = LINE('',#17657,#3528) ;
#2758 = LINE('',#17661,#3529) ;
#2759 = LINE('',#17665,#3530) ;
#2760 = LINE('',#17669,#3531) ;
#2761 = LINE('',#17673,#3532) ;
#2762 = LINE('',#17677,#3533) ;
#2763 = LINE('',#17681,#3534) ;
#2764 = LINE('',#17685,#3535) ;
#2765 = LINE('',#17689,#3536) ;
#2766 = LINE('',#17693,#3537) ;
#2767 = LINE('',#17697,#3538) ;
#2768 = LINE('',#17701,#3539) ;
#2769 = LINE('',#17705,#3540) ;
#2770 = LINE('',#17709,#3541) ;
#2771 = LINE('',#17713,#3542) ;
#2772 = LINE('',#17717,#3543) ;
#2773 = LINE('',#17721,#3544) ;
#2774 = LINE('',#17725,#3545) ;
#2775 = LINE('',#17729,#3546) ;
#2776 = LINE('',#17733,#3547) ;
#2777 = LINE('',#17735,#3548) ;
#2778 = LINE('',#17743,#3549) ;
#2779 = LINE('',#17749,#3550) ;
#2780 = LINE('',#17989,#3551) ;
#2781 = LINE('',#17990,#3552) ;
#2782 = LINE('',#17992,#3553) ;
#2783 = LINE('',#17996,#3554) ;
#2784 = LINE('',#17997,#3555) ;
#2785 = LINE('',#17999,#3556) ;
#2786 = LINE('',#18003,#3557) ;
#2787 = LINE('',#18004,#3558) ;
#2788 = LINE('',#18006,#3559) ;
#2789 = LINE('',#18010,#3560) ;
#2790 = LINE('',#18011,#3561) ;
#2791 = LINE('',#18013,#3562) ;
#2792 = LINE('',#18017,#3563) ;
#2793 = LINE('',#18018,#3564) ;
#2794 = LINE('',#18020,#3565) ;
#2795 = LINE('',#18024,#3566) ;
#2796 = LINE('',#18025,#3567) ;
#2797 = LINE('',#18027,#3568) ;
#2798 = LINE('',#18031,#3569) ;
#2799 = LINE('',#18032,#3570) ;
#2800 = LINE('',#18034,#3571) ;
#2801 = LINE('',#18038,#3572) ;
#2802 = LINE('',#18039,#3573) ;
#2803 = LINE('',#18041,#3574) ;
#2804 = LINE('',#18045,#3575) ;
#2805 = LINE('',#18046,#3576) ;
#2806 = LINE('',#18048,#3577) ;
#2807 = LINE('',#18052,#3578) ;
#2808 = LINE('',#18053,#3579) ;
#2809 = LINE('',#18055,#3580) ;
#2810 = LINE('',#18059,#3581) ;
#2811 = LINE('',#18060,#3582) ;
#2812 = LINE('',#18062,#3583) ;
#2813 = LINE('',#18066,#3584) ;
#2814 = LINE('',#18067,#3585) ;
#2815 = LINE('',#18069,#3586) ;
#2816 = LINE('',#18073,#3587) ;
#2817 = LINE('',#18074,#3588) ;
#2818 = LINE('',#18076,#3589) ;
#2819 = LINE('',#18080,#3590) ;
#2820 = LINE('',#18081,#3591) ;
#2821 = LINE('',#18083,#3592) ;
#2822 = LINE('',#18087,#3593) ;
#2823 = LINE('',#18088,#3594) ;
#2824 = LINE('',#18090,#3595) ;
#2825 = LINE('',#18094,#3596) ;
#2826 = LINE('',#18095,#3597) ;
#2827 = LINE('',#18097,#3598) ;
#2828 = LINE('',#18101,#3599) ;
#2829 = LINE('',#18102,#3600) ;
#2830 = LINE('',#18104,#3601) ;
#2831 = LINE('',#18108,#3602) ;
#2832 = LINE('',#18109,#3603) ;
#2833 = LINE('',#18111,#3604) ;
#2834 = LINE('',#18115,#3605) ;
#2835 = LINE('',#18116,#3606) ;
#2836 = LINE('',#18118,#3607) ;
#2837 = LINE('',#18122,#3608) ;
#2838 = LINE('',#18123,#3609) ;
#2839 = LINE('',#18125,#3610) ;
#2840 = LINE('',#18129,#3611) ;
#2841 = LINE('',#18130,#3612) ;
#2842 = LINE('',#18132,#3613) ;
#2843 = LINE('',#18136,#3614) ;
#2844 = LINE('',#18137,#3615) ;
#2845 = LINE('',#18139,#3616) ;
#2846 = LINE('',#18143,#3617) ;
#2847 = LINE('',#18144,#3618) ;
#2848 = LINE('',#18146,#3619) ;
#2849 = LINE('',#18150,#3620) ;
#2850 = LINE('',#18151,#3621) ;
#2851 = LINE('',#18153,#3622) ;
#2852 = LINE('',#18157,#3623) ;
#2853 = LINE('',#18158,#3624) ;
#2854 = LINE('',#18160,#3625) ;
#2855 = LINE('',#18164,#3626) ;
#2856 = LINE('',#18165,#3627) ;
#2857 = LINE('',#18167,#3628) ;
#2858 = LINE('',#18171,#3629) ;
#2859 = LINE('',#18172,#3630) ;
#2860 = LINE('',#18174,#3631) ;
#2861 = LINE('',#18178,#3632) ;
#2862 = LINE('',#18179,#3633) ;
#2863 = LINE('',#18181,#3634) ;
#2864 = LINE('',#18185,#3635) ;
#2865 = LINE('',#18186,#3636) ;
#2866 = LINE('',#18188,#3637) ;
#2867 = LINE('',#18192,#3638) ;
#2868 = LINE('',#18193,#3639) ;
#2869 = LINE('',#18195,#3640) ;
#2870 = LINE('',#18199,#3641) ;
#2871 = LINE('',#18200,#3642) ;
#2872 = LINE('',#18202,#3643) ;
#2873 = LINE('',#18206,#3644) ;
#2874 = LINE('',#18207,#3645) ;
#2875 = LINE('',#18209,#3646) ;
#2876 = LINE('',#18213,#3647) ;
#2877 = LINE('',#18214,#3648) ;
#2878 = LINE('',#18216,#3649) ;
#2879 = LINE('',#18220,#3650) ;
#2880 = LINE('',#18221,#3651) ;
#2881 = LINE('',#18223,#3652) ;
#2882 = LINE('',#18232,#3653) ;
#2883 = LINE('',#18294,#3654) ;
#2884 = LINE('',#18296,#3655) ;
#2885 = LINE('',#18300,#3656) ;
#2886 = LINE('',#18302,#3657) ;
#2887 = LINE('',#18306,#3658) ;
#2888 = LINE('',#18309,#3659) ;
#2889 = LINE('',#18312,#3660) ;
#2890 = LINE('',#18314,#3661) ;
#2891 = LINE('',#18318,#3662) ;
#2892 = LINE('',#18321,#3663) ;
#2893 = LINE('',#18324,#3664) ;
#2894 = LINE('',#18327,#3665) ;
#2895 = LINE('',#18329,#3666) ;
#2896 = LINE('',#18331,#3667) ;
#2897 = LINE('',#18333,#3668) ;
#2898 = LINE('',#18334,#3669) ;
#2899 = LINE('',#18336,#3670) ;
#2900 = LINE('',#18338,#3671) ;
#2901 = LINE('',#18339,#3672) ;
#2902 = LINE('',#18341,#3673) ;
#2903 = LINE('',#18343,#3674) ;
#2904 = LINE('',#18344,#3675) ;
#2905 = LINE('',#18348,#3676) ;
#2906 = LINE('',#18351,#3677) ;
#2907 = LINE('',#18353,#3678) ;
#2908 = LINE('',#18356,#3679) ;
#2909 = LINE('',#18366,#3680) ;
#2910 = LINE('',#18369,#3681) ;
#2911 = LINE('',#18373,#3682) ;
#2912 = LINE('',#18375,#3683) ;
#2913 = LINE('',#18377,#3684) ;
#2914 = LINE('',#18384,#3685) ;
#2915 = LINE('',#18390,#3686) ;
#2916 = LINE('',#18397,#3687) ;
#2917 = LINE('',#18399,#3688) ;
#2918 = LINE('',#18401,#3689) ;
#2919 = LINE('',#18403,#3690) ;
#2920 = LINE('',#18404,#3691) ;
#2921 = LINE('',#18409,#3692) ;
#2922 = LINE('',#18413,#3693) ;
#2923 = LINE('',#18415,#3694) ;
#2924 = LINE('',#18416,#3695) ;
#2925 = LINE('',#18422,#3696) ;
#2926 = LINE('',#18424,#3697) ;
#2927 = LINE('',#18425,#3698) ;
#2928 = LINE('',#18428,#3699) ;
#2929 = LINE('',#18430,#3700) ;
#2930 = LINE('',#18431,#3701) ;
#2931 = LINE('',#18439,#3702) ;
#2932 = LINE('',#18443,#3703) ;
#2933 = LINE('',#18445,#3704) ;
#2934 = LINE('',#18447,#3705) ;
#2935 = LINE('',#18449,#3706) ;
#2936 = LINE('',#18453,#3707) ;
#2937 = LINE('',#18454,#3708) ;
#2938 = LINE('',#18460,#3709) ;
#2939 = LINE('',#18463,#3710) ;
#2940 = LINE('',#18465,#3711) ;
#2941 = LINE('',#18466,#3712) ;
#2942 = LINE('',#18470,#3713) ;
#2943 = LINE('',#18473,#3714) ;
#2944 = LINE('',#18474,#3715) ;
#2945 = LINE('',#18477,#3716) ;
#2946 = LINE('',#18482,#3717) ;
#2947 = LINE('',#18488,#3718) ;
#2948 = LINE('',#18493,#3719) ;
#2949 = LINE('',#18495,#3720) ;
#2950 = LINE('',#18497,#3721) ;
#2951 = LINE('',#18498,#3722) ;
#2952 = LINE('',#18501,#3723) ;
#2953 = LINE('',#18503,#3724) ;
#2954 = LINE('',#18504,#3725) ;
#2955 = LINE('',#18507,#3726) ;
#2956 = LINE('',#18509,#3727) ;
#2957 = LINE('',#18510,#3728) ;
#2958 = LINE('',#18512,#3729) ;
#2959 = LINE('',#18513,#3730) ;
#2960 = LINE('',#18521,#3731) ;
#2961 = LINE('',#18527,#3732) ;
#2962 = LINE('',#18532,#3733) ;
#2963 = LINE('',#18534,#3734) ;
#2964 = LINE('',#18537,#3735) ;
#2965 = LINE('',#18542,#3736) ;
#2966 = LINE('',#18544,#3737) ;
#2967 = LINE('',#18545,#3738) ;
#2968 = LINE('',#18548,#3739) ;
#2969 = LINE('',#18552,#3740) ;
#2970 = LINE('',#18554,#3741) ;
#2971 = LINE('',#18555,#3742) ;
#2972 = LINE('',#18559,#3743) ;
#2973 = LINE('',#18563,#3744) ;
#2974 = LINE('',#18565,#3745) ;
#2975 = LINE('',#18568,#3746) ;
#2976 = LINE('',#18573,#3747) ;
#2977 = LINE('',#18575,#3748) ;
#2978 = LINE('',#18576,#3749) ;
#2979 = LINE('',#18579,#3750) ;
#2980 = LINE('',#18583,#3751) ;
#2981 = LINE('',#18585,#3752) ;
#2982 = LINE('',#18586,#3753) ;
#2983 = LINE('',#18590,#3754) ;
#2984 = LINE('',#18594,#3755) ;
#2985 = LINE('',#18596,#3756) ;
#2986 = LINE('',#18598,#3757) ;
#2987 = LINE('',#18599,#3758) ;
#2988 = LINE('',#18602,#3759) ;
#2989 = LINE('',#18604,#3760) ;
#2990 = LINE('',#18605,#3761) ;
#2991 = LINE('',#18608,#3762) ;
#2992 = LINE('',#18610,#3763) ;
#2993 = LINE('',#18611,#3764) ;
#2994 = LINE('',#18613,#3765) ;
#2995 = LINE('',#18614,#3766) ;
#2996 = LINE('',#18626,#3767) ;
#2997 = LINE('',#18633,#3768) ;
#2998 = LINE('',#18637,#3769) ;
#2999 = LINE('',#18641,#3770) ;
#3000 = LINE('',#18645,#3771) ;
#3001 = LINE('',#18649,#3772) ;
#3002 = LINE('',#18656,#3773) ;
#3003 = LINE('',#18661,#3774) ;
#3004 = VECTOR('',#10723,1.12500000000001) ;
#3005 = VECTOR('',#10728,10.) ;
#3006 = VECTOR('',#10729,10.) ;
#3007 = VECTOR('',#10730,10.) ;
#3008 = VECTOR('',#10731,10.) ;
#3009 = VECTOR('',#10736,1.05) ;
#3010 = VECTOR('',#10743,1.12500000000001) ;
#3011 = VECTOR('',#10748,10.) ;
#3012 = VECTOR('',#10749,10.) ;
#3013 = VECTOR('',#10750,10.) ;
#3014 = VECTOR('',#10751,10.) ;
#3015 = VECTOR('',#10756,1.05) ;
#3016 = VECTOR('',#10763,1.12500000000001) ;
#3017 = VECTOR('',#10768,10.) ;
#3018 = VECTOR('',#10769,10.) ;
#3019 = VECTOR('',#10770,10.) ;
#3020 = VECTOR('',#10771,10.) ;
#3021 = VECTOR('',#10776,1.05) ;
#3022 = VECTOR('',#10783,1.12500000000001) ;
#3023 = VECTOR('',#10788,10.) ;
#3024 = VECTOR('',#10789,10.) ;
#3025 = VECTOR('',#10790,10.) ;
#3026 = VECTOR('',#10791,10.) ;
#3027 = VECTOR('',#10796,1.05) ;
#3028 = VECTOR('',#10801,1.125) ;
#3029 = VECTOR('',#10806,1.05) ;
#3030 = VECTOR('',#10813,1.125) ;
#3031 = VECTOR('',#10818,1.05) ;
#3032 = VECTOR('',#10825,1.125) ;
#3033 = VECTOR('',#10830,1.05) ;
#3034 = VECTOR('',#10835,1.125) ;
#3035 = VECTOR('',#10840,1.05) ;
#3036 = VECTOR('',#10845,1.04999999999999) ;
#3037 = VECTOR('',#10848,1.05) ;
#3038 = VECTOR('',#10851,1.04999999999999) ;
#3039 = VECTOR('',#10854,1.05) ;
#3040 = VECTOR('',#10861,2.05) ;
#3041 = VECTOR('',#10866,1.05) ;
#3042 = VECTOR('',#10873,2.05) ;
#3043 = VECTOR('',#10878,1.05) ;
#3044 = VECTOR('',#10881,1.15) ;
#3045 = VECTOR('',#10886,2.95) ;
#3046 = VECTOR('',#10893,1.15) ;
#3047 = VECTOR('',#10898,2.95) ;
#3048 = VECTOR('',#10907,2.05) ;
#3049 = VECTOR('',#10914,2.05) ;
#3050 = VECTOR('',#10919,10.) ;
#3051 = VECTOR('',#10922,10.) ;
#3052 = VECTOR('',#10927,10.) ;
#3053 = VECTOR('',#10930,10.) ;
#3054 = VECTOR('',#10935,10.) ;
#3055 = VECTOR('',#10936,10.) ;
#3056 = VECTOR('',#10937,10.) ;
#3057 = VECTOR('',#10942,10.) ;
#3058 = VECTOR('',#10943,10.) ;
#3059 = VECTOR('',#10944,10.) ;
#3060 = VECTOR('',#10947,10.) ;
#3061 = VECTOR('',#10948,10.) ;
#3062 = VECTOR('',#10949,10.) ;
#3063 = VECTOR('',#10954,10.) ;
#3064 = VECTOR('',#10955,10.) ;
#3065 = VECTOR('',#10956,10.) ;
#3066 = VECTOR('',#10959,10.) ;
#3067 = VECTOR('',#10960,10.) ;
#3068 = VECTOR('',#10961,10.) ;
#3069 = VECTOR('',#10962,10.) ;
#3070 = VECTOR('',#10965,10.) ;
#3071 = VECTOR('',#10966,10.) ;
#3072 = VECTOR('',#10967,10.) ;
#3073 = VECTOR('',#10968,10.) ;
#3074 = VECTOR('',#10969,10.) ;
#3075 = VECTOR('',#10972,10.) ;
#3076 = VECTOR('',#10973,10.) ;
#3077 = VECTOR('',#10974,10.) ;
#3078 = VECTOR('',#10975,10.) ;
#3079 = VECTOR('',#10976,10.) ;
#3080 = VECTOR('',#10977,10.) ;
#3081 = VECTOR('',#10978,10.) ;
#3082 = VECTOR('',#10979,10.) ;
#3083 = VECTOR('',#10980,10.) ;
#3084 = VECTOR('',#10981,10.) ;
#3085 = VECTOR('',#10982,10.) ;
#3086 = VECTOR('',#10983,10.) ;
#3087 = VECTOR('',#10984,10.) ;
#3088 = VECTOR('',#10985,10.) ;
#3089 = VECTOR('',#10986,10.) ;
#3090 = VECTOR('',#10987,10.) ;
#3091 = VECTOR('',#10988,10.) ;
#3092 = VECTOR('',#10989,10.) ;
#3093 = VECTOR('',#10992,10.) ;
#3094 = VECTOR('',#10993,10.) ;
#3095 = VECTOR('',#10994,10.) ;
#3096 = VECTOR('',#10997,10.) ;
#3097 = VECTOR('',#10998,10.) ;
#3098 = VECTOR('',#10999,10.) ;
#3099 = VECTOR('',#11000,10.) ;
#3100 = VECTOR('',#11005,3.99999999999999) ;
#3101 = VECTOR('',#11008,10.) ;
#3102 = VECTOR('',#11015,10.) ;
#3103 = VECTOR('',#11022,10.) ;
#3104 = VECTOR('',#11027,10.) ;
#3105 = VECTOR('',#11028,10.) ;
#3106 = VECTOR('',#11029,10.) ;
#3107 = VECTOR('',#11030,10.) ;
#3108 = VECTOR('',#11031,10.) ;
#3109 = VECTOR('',#11032,10.) ;
#3110 = VECTOR('',#11033,10.) ;
#3111 = VECTOR('',#11034,10.) ;
#3112 = VECTOR('',#11035,10.) ;
#3113 = VECTOR('',#11036,10.) ;
#3114 = VECTOR('',#11037,10.) ;
#3115 = VECTOR('',#11038,10.) ;
#3116 = VECTOR('',#11039,10.) ;
#3117 = VECTOR('',#11040,10.) ;
#3118 = VECTOR('',#11041,10.) ;
#3119 = VECTOR('',#11042,10.) ;
#3120 = VECTOR('',#11043,10.) ;
#3121 = VECTOR('',#11050,10.) ;
#3122 = VECTOR('',#11053,10.) ;
#3123 = VECTOR('',#11054,10.) ;
#3124 = VECTOR('',#11063,10.) ;
#3125 = VECTOR('',#11064,10.) ;
#3126 = VECTOR('',#11065,10.) ;
#3127 = VECTOR('',#11066,10.) ;
#3128 = VECTOR('',#11069,10.) ;
#3129 = VECTOR('',#11070,10.) ;
#3130 = VECTOR('',#11071,10.) ;
#3131 = VECTOR('',#11074,10.) ;
#3132 = VECTOR('',#11075,10.) ;
#3133 = VECTOR('',#11080,3.99999999999999) ;
#3134 = VECTOR('',#11097,10.) ;
#3135 = VECTOR('',#11100,10.) ;
#3136 = VECTOR('',#11101,10.) ;
#3137 = VECTOR('',#11110,10.) ;
#3138 = VECTOR('',#11111,10.) ;
#3139 = VECTOR('',#11112,10.) ;
#3140 = VECTOR('',#11113,10.) ;
#3141 = VECTOR('',#11116,10.) ;
#3142 = VECTOR('',#11117,10.) ;
#3143 = VECTOR('',#11118,10.) ;
#3144 = VECTOR('',#11121,10.) ;
#3145 = VECTOR('',#11122,10.) ;
#3146 = VECTOR('',#11125,10.) ;
#3147 = VECTOR('',#11126,10.) ;
#3148 = VECTOR('',#11127,10.) ;
#3149 = VECTOR('',#11130,10.) ;
#3150 = VECTOR('',#11131,10.) ;
#3151 = VECTOR('',#11132,10.) ;
#3152 = VECTOR('',#11135,10.) ;
#3153 = VECTOR('',#11136,10.) ;
#3154 = VECTOR('',#11139,10.) ;
#3155 = VECTOR('',#11142,10.) ;
#3156 = VECTOR('',#11143,10.) ;
#3157 = VECTOR('',#11144,10.) ;
#3158 = VECTOR('',#11147,10.) ;
#3159 = VECTOR('',#11148,10.) ;
#3160 = VECTOR('',#11151,10.) ;
#3161 = VECTOR('',#11152,10.) ;
#3162 = VECTOR('',#11155,10.) ;
#3163 = VECTOR('',#11156,10.) ;
#3164 = VECTOR('',#11159,10.) ;
#3165 = VECTOR('',#11160,10.) ;
#3166 = VECTOR('',#11161,10.) ;
#3167 = VECTOR('',#11162,10.) ;
#3168 = VECTOR('',#11163,10.) ;
#3169 = VECTOR('',#11164,10.) ;
#3170 = VECTOR('',#11167,10.) ;
#3171 = VECTOR('',#11168,10.) ;
#3172 = VECTOR('',#11169,10.) ;
#3173 = VECTOR('',#11172,10.) ;
#3174 = VECTOR('',#11173,10.) ;
#3175 = VECTOR('',#11176,10.) ;
#3176 = VECTOR('',#11177,10.) ;
#3177 = VECTOR('',#11180,10.) ;
#3178 = VECTOR('',#11181,10.) ;
#3179 = VECTOR('',#11182,10.) ;
#3180 = VECTOR('',#11185,10.) ;
#3181 = VECTOR('',#11188,10.) ;
#3182 = VECTOR('',#11191,10.) ;
#3183 = VECTOR('',#11194,10.) ;
#3184 = VECTOR('',#11197,10.) ;
#3185 = VECTOR('',#11198,10.) ;
#3186 = VECTOR('',#11201,10.) ;
#3187 = VECTOR('',#11202,10.) ;
#3188 = VECTOR('',#11205,10.) ;
#3189 = VECTOR('',#11208,10.) ;
#3190 = VECTOR('',#11213,10.) ;
#3191 = VECTOR('',#11216,10.) ;
#3192 = VECTOR('',#11225,2.05) ;
#3193 = VECTOR('',#11232,2.05) ;
#3194 = VECTOR('',#11237,10.) ;
#3195 = VECTOR('',#11238,10.) ;
#3196 = VECTOR('',#11239,10.) ;
#3197 = VECTOR('',#11240,10.) ;
#3198 = VECTOR('',#11243,10.) ;
#3199 = VECTOR('',#11244,10.) ;
#3200 = VECTOR('',#11245,10.) ;
#3201 = VECTOR('',#11246,10.) ;
#3202 = VECTOR('',#11247,10.) ;
#3203 = VECTOR('',#11250,10.) ;
#3204 = VECTOR('',#11251,10.) ;
#3205 = VECTOR('',#11252,10.) ;
#3206 = VECTOR('',#11255,10.) ;
#3207 = VECTOR('',#11258,10.) ;
#3208 = VECTOR('',#11259,10.) ;
#3209 = VECTOR('',#11260,10.) ;
#3210 = VECTOR('',#11265,10.) ;
#3211 = VECTOR('',#11272,10.) ;
#3212 = VECTOR('',#11279,10.) ;
#3213 = VECTOR('',#11282,10.) ;
#3214 = VECTOR('',#11285,10.) ;
#3215 = VECTOR('',#11288,10.) ;
#3216 = VECTOR('',#11289,10.) ;
#3217 = VECTOR('',#11292,10.) ;
#3218 = VECTOR('',#11293,10.) ;
#3219 = VECTOR('',#11296,10.) ;
#3220 = VECTOR('',#11299,10.) ;
#3221 = VECTOR('',#11302,10.) ;
#3222 = VECTOR('',#11305,10.) ;
#3223 = VECTOR('',#11306,10.) ;
#3224 = VECTOR('',#11307,10.) ;
#3225 = VECTOR('',#11308,10.) ;
#3226 = VECTOR('',#11311,10.) ;
#3227 = VECTOR('',#11312,10.) ;
#3228 = VECTOR('',#11313,10.) ;
#3229 = VECTOR('',#11316,10.) ;
#3230 = VECTOR('',#11317,10.) ;
#3231 = VECTOR('',#11318,10.) ;
#3232 = VECTOR('',#11319,10.) ;
#3233 = VECTOR('',#11322,10.) ;
#3234 = VECTOR('',#11325,10.) ;
#3235 = VECTOR('',#11326,10.) ;
#3236 = VECTOR('',#11331,10.) ;
#3237 = VECTOR('',#11334,10.) ;
#3238 = VECTOR('',#11341,10.) ;
#3239 = VECTOR('',#11344,10.) ;
#3240 = VECTOR('',#11357,10.) ;
#3241 = VECTOR('',#11358,10.) ;
#3242 = VECTOR('',#11371,10.) ;
#3243 = VECTOR('',#11372,10.) ;
#3244 = VECTOR('',#11385,10.) ;
#3245 = VECTOR('',#11386,10.) ;
#3246 = VECTOR('',#11395,10.) ;
#3247 = VECTOR('',#11396,10.) ;
#3248 = VECTOR('',#11399,10.) ;
#3249 = VECTOR('',#11402,10.) ;
#3250 = VECTOR('',#11405,10.) ;
#3251 = VECTOR('',#11410,10.) ;
#3252 = VECTOR('',#11411,10.) ;
#3253 = VECTOR('',#11412,10.) ;
#3254 = VECTOR('',#11415,10.) ;
#3255 = VECTOR('',#11420,10.) ;
#3256 = VECTOR('',#11423,10.) ;
#3257 = VECTOR('',#11426,10.) ;
#3258 = VECTOR('',#11427,10.) ;
#3259 = VECTOR('',#11436,10.) ;
#3260 = VECTOR('',#11439,10.) ;
#3261 = VECTOR('',#11442,10.) ;
#3262 = VECTOR('',#11451,2.5) ;
#3263 = VECTOR('',#11458,1.5) ;
#3264 = VECTOR('',#11465,2.05) ;
#3265 = VECTOR('',#11472,2.05) ;
#3266 = VECTOR('',#11477,10.) ;
#3267 = VECTOR('',#11478,10.) ;
#3268 = VECTOR('',#11479,10.) ;
#3269 = VECTOR('',#11480,10.) ;
#3270 = VECTOR('',#11487,10.) ;
#3271 = VECTOR('',#11490,10.) ;
#3272 = VECTOR('',#11491,10.) ;
#3273 = VECTOR('',#11492,10.) ;
#3274 = VECTOR('',#11507,1.5) ;
#3275 = VECTOR('',#11514,2.05) ;
#3276 = VECTOR('',#11521,2.05) ;
#3277 = VECTOR('',#11526,10.) ;
#3278 = VECTOR('',#11527,10.) ;
#3279 = VECTOR('',#11528,10.) ;
#3280 = VECTOR('',#11529,10.) ;
#3281 = VECTOR('',#11536,10.) ;
#3282 = VECTOR('',#11539,10.) ;
#3283 = VECTOR('',#11540,10.) ;
#3284 = VECTOR('',#11541,10.) ;
#3285 = VECTOR('',#11558,2.5) ;
#3286 = VECTOR('',#11565,2.5) ;
#3287 = VECTOR('',#11572,2.05) ;
#3288 = VECTOR('',#11579,1.5) ;
#3289 = VECTOR('',#11586,2.05) ;
#3290 = VECTOR('',#11591,10.) ;
#3291 = VECTOR('',#11592,10.) ;
#3292 = VECTOR('',#11593,10.) ;
#3293 = VECTOR('',#11594,10.) ;
#3294 = VECTOR('',#11601,10.) ;
#3295 = VECTOR('',#11604,10.) ;
#3296 = VECTOR('',#11605,10.) ;
#3297 = VECTOR('',#11606,10.) ;
#3298 = VECTOR('',#11621,1.5) ;
#3299 = VECTOR('',#11628,2.05) ;
#3300 = VECTOR('',#11635,2.05) ;
#3301 = VECTOR('',#11640,10.) ;
#3302 = VECTOR('',#11641,10.) ;
#3303 = VECTOR('',#11642,10.) ;
#3304 = VECTOR('',#11643,10.) ;
#3305 = VECTOR('',#11650,10.) ;
#3306 = VECTOR('',#11653,10.) ;
#3307 = VECTOR('',#11654,10.) ;
#3308 = VECTOR('',#11655,10.) ;
#3309 = VECTOR('',#11670,3.) ;
#3310 = VECTOR('',#11675,3.) ;
#3311 = VECTOR('',#11684,2.05) ;
#3312 = VECTOR('',#11693,4.6) ;
#3313 = VECTOR('',#11702,2.09999999999999) ;
#3314 = VECTOR('',#11713,4.99999999999999) ;
#3315 = VECTOR('',#11720,1.99999999999999) ;
#3316 = VECTOR('',#11733,3.5) ;
#3317 = VECTOR('',#11736,10.) ;
#3318 = VECTOR('',#11743,2.55) ;
#3319 = VECTOR('',#11750,10.) ;
#3320 = VECTOR('',#11771,2.) ;
#3321 = VECTOR('',#11780,4.50000000000001) ;
#3322 = VECTOR('',#11787,10.) ;
#3323 = VECTOR('',#11790,10.) ;
#3324 = VECTOR('',#11795,10.) ;
#3325 = VECTOR('',#11796,10.) ;
#3326 = VECTOR('',#11797,10.) ;
#3327 = VECTOR('',#11798,10.) ;
#3328 = VECTOR('',#11799,10.) ;
#3329 = VECTOR('',#11800,10.) ;
#3330 = VECTOR('',#11801,10.) ;
#3331 = VECTOR('',#11804,10.) ;
#3332 = VECTOR('',#11805,10.) ;
#3333 = VECTOR('',#11808,10.) ;
#3334 = VECTOR('',#11809,10.) ;
#3335 = VECTOR('',#11814,10.) ;
#3336 = VECTOR('',#11815,10.) ;
#3337 = VECTOR('',#11820,10.) ;
#3338 = VECTOR('',#11823,10.) ;
#3339 = VECTOR('',#11824,10.) ;
#3340 = VECTOR('',#11825,10.) ;
#3341 = VECTOR('',#11826,10.) ;
#3342 = VECTOR('',#11829,10.) ;
#3343 = VECTOR('',#11844,10.) ;
#3344 = VECTOR('',#11849,5.) ;
#3345 = VECTOR('',#11852,10.) ;
#3346 = VECTOR('',#11853,10.) ;
#3347 = VECTOR('',#11858,10.) ;
#3348 = VECTOR('',#11859,10.) ;
#3349 = VECTOR('',#11860,10.) ;
#3350 = VECTOR('',#11861,10.) ;
#3351 = VECTOR('',#11862,10.) ;
#3352 = VECTOR('',#11865,10.) ;
#3353 = VECTOR('',#11866,10.) ;
#3354 = VECTOR('',#11867,10.) ;
#3355 = VECTOR('',#11870,10.) ;
#3356 = VECTOR('',#11871,10.) ;
#3357 = VECTOR('',#11874,10.) ;
#3358 = VECTOR('',#11875,10.) ;
#3359 = VECTOR('',#11878,10.) ;
#3360 = VECTOR('',#11885,10.) ;
#3361 = VECTOR('',#11886,10.) ;
#3362 = VECTOR('',#11887,10.) ;
#3363 = VECTOR('',#11888,10.) ;
#3364 = VECTOR('',#11891,10.) ;
#3365 = VECTOR('',#11892,10.) ;
#3366 = VECTOR('',#11893,10.) ;
#3367 = VECTOR('',#11896,10.) ;
#3368 = VECTOR('',#11897,10.) ;
#3369 = VECTOR('',#11898,10.) ;
#3370 = VECTOR('',#11901,10.) ;
#3371 = VECTOR('',#11902,10.) ;
#3372 = VECTOR('',#11903,10.) ;
#3373 = VECTOR('',#11904,10.) ;
#3374 = VECTOR('',#11905,10.) ;
#3375 = VECTOR('',#11908,10.) ;
#3376 = VECTOR('',#11911,10.) ;
#3377 = VECTOR('',#11914,10.) ;
#3378 = VECTOR('',#11921,10.) ;
#3379 = VECTOR('',#11922,10.) ;
#3380 = VECTOR('',#11925,2.05) ;
#3381 = VECTOR('',#11930,10.) ;
#3382 = VECTOR('',#11935,10.) ;
#3383 = VECTOR('',#11936,10.) ;
#3384 = VECTOR('',#11947,1.05) ;
#3385 = VECTOR('',#11950,1.05) ;
#3386 = VECTOR('',#11955,2.05) ;
#3387 = VECTOR('',#11962,10.) ;
#3388 = VECTOR('',#11963,10.) ;
#3389 = VECTOR('',#11964,10.) ;
#3390 = VECTOR('',#11965,10.) ;
#3391 = VECTOR('',#11966,10.) ;
#3392 = VECTOR('',#11969,10.) ;
#3393 = VECTOR('',#11970,10.) ;
#3394 = VECTOR('',#11971,10.) ;
#3395 = VECTOR('',#11974,10.) ;
#3396 = VECTOR('',#11975,10.) ;
#3397 = VECTOR('',#11976,10.) ;
#3398 = VECTOR('',#11979,10.) ;
#3399 = VECTOR('',#11980,10.) ;
#3400 = VECTOR('',#11983,10.) ;
#3401 = VECTOR('',#11986,10.) ;
#3402 = VECTOR('',#11987,10.) ;
#3403 = VECTOR('',#11996,2.85) ;
#3404 = VECTOR('',#11997,2.85) ;
#3405 = VECTOR('',#12012,2.85) ;
#3406 = VECTOR('',#12027,2.85) ;
#3407 = VECTOR('',#12028,2.85) ;
#3408 = VECTOR('',#12041,2.05) ;
#3409 = VECTOR('',#12046,10.) ;
#3410 = VECTOR('',#12047,10.) ;
#3411 = VECTOR('',#12048,10.) ;
#3412 = VECTOR('',#12049,10.) ;
#3413 = VECTOR('',#12056,10.) ;
#3414 = VECTOR('',#12059,10.) ;
#3415 = VECTOR('',#12060,10.) ;
#3416 = VECTOR('',#12061,10.) ;
#3417 = VECTOR('',#12082,2.9) ;
#3418 = VECTOR('',#12087,3.) ;
#3419 = VECTOR('',#12096,2.) ;
#3420 = VECTOR('',#12105,1.59999999999999) ;
#3421 = VECTOR('',#12114,2.) ;
#3422 = VECTOR('',#12119,1.875) ;
#3423 = VECTOR('',#12126,10.) ;
#3424 = VECTOR('',#12127,10.) ;
#3425 = VECTOR('',#12128,10.) ;
#3426 = VECTOR('',#12129,10.) ;
#3427 = VECTOR('',#12132,10.) ;
#3428 = VECTOR('',#12133,10.) ;
#3429 = VECTOR('',#12134,10.) ;
#3430 = VECTOR('',#12135,10.) ;
#3431 = VECTOR('',#12138,10.) ;
#3432 = VECTOR('',#12139,10.) ;
#3433 = VECTOR('',#12140,10.) ;
#3434 = VECTOR('',#12143,10.) ;
#3435 = VECTOR('',#12144,10.) ;
#3436 = VECTOR('',#12145,10.) ;
#3437 = VECTOR('',#12172,3.85000000000001) ;
#3438 = VECTOR('',#12177,4.) ;
#3439 = VECTOR('',#12182,3.85000000000001) ;
#3440 = VECTOR('',#12191,1.5) ;
#3441 = VECTOR('',#12196,1.40000000000001) ;
#3442 = VECTOR('',#12203,0.999999999999996) ;
#3443 = VECTOR('',#12208,0.999999999999996) ;
#3444 = VECTOR('',#12211,0.999999999999996) ;
#3445 = VECTOR('',#12214,0.999999999999996) ;
#3446 = VECTOR('',#12217,0.999999999999996) ;
#3447 = VECTOR('',#12220,0.999999999999996) ;
#3448 = VECTOR('',#12223,0.999999999999996) ;
#3449 = VECTOR('',#12226,0.999999999999996) ;
#3450 = VECTOR('',#12229,0.999999999999996) ;
#3451 = VECTOR('',#12232,0.999999999999996) ;
#3452 = VECTOR('',#12235,0.999999999999996) ;
#3453 = VECTOR('',#12238,0.999999999999996) ;
#3454 = VECTOR('',#12241,0.999999999999996) ;
#3455 = VECTOR('',#12244,0.999999999999996) ;
#3456 = VECTOR('',#12247,0.739000000000001) ;
#3457 = VECTOR('',#12252,0.739000000000001) ;
#3458 = VECTOR('',#12255,0.739000000000001) ;
#3459 = VECTOR('',#12258,0.739000000000001) ;
#3460 = VECTOR('',#12261,0.739000000000001) ;
#3461 = VECTOR('',#12264,0.739000000000001) ;
#3462 = VECTOR('',#12267,0.739000000000001) ;
#3463 = VECTOR('',#12270,0.739000000000001) ;
#3464 = VECTOR('',#12273,0.739000000000001) ;
#3465 = VECTOR('',#12276,0.739000000000001) ;
#3466 = VECTOR('',#12279,0.739000000000001) ;
#3467 = VECTOR('',#12282,0.739000000000001) ;
#3468 = VECTOR('',#12285,0.739000000000001) ;
#3469 = VECTOR('',#12288,0.739000000000001) ;
#3470 = VECTOR('',#12321,0.79175) ;
#3471 = VECTOR('',#12330,10.) ;
#3472 = VECTOR('',#12331,10.) ;
#3473 = VECTOR('',#12334,10.) ;
#3474 = VECTOR('',#12335,10.) ;
#3475 = VECTOR('',#12338,10.) ;
#3476 = VECTOR('',#12343,10.) ;
#3477 = VECTOR('',#12346,10.) ;
#3478 = VECTOR('',#12349,10.) ;
#3479 = VECTOR('',#12352,10.) ;
#3480 = VECTOR('',#12355,10.) ;
#3481 = VECTOR('',#12358,10.) ;
#3482 = VECTOR('',#12361,10.) ;
#3483 = VECTOR('',#12364,10.) ;
#3484 = VECTOR('',#12367,10.) ;
#3485 = VECTOR('',#12370,10.) ;
#3486 = VECTOR('',#12373,10.) ;
#3487 = VECTOR('',#12376,10.) ;
#3488 = VECTOR('',#12379,10.) ;
#3489 = VECTOR('',#12382,10.) ;
#3490 = VECTOR('',#12385,10.) ;
#3491 = VECTOR('',#12388,10.) ;
#3492 = VECTOR('',#12391,10.) ;
#3493 = VECTOR('',#12394,10.) ;
#3494 = VECTOR('',#12397,10.) ;
#3495 = VECTOR('',#12400,10.) ;
#3496 = VECTOR('',#12403,10.) ;
#3497 = VECTOR('',#12406,10.) ;
#3498 = VECTOR('',#12409,10.) ;
#3499 = VECTOR('',#12412,10.) ;
#3500 = VECTOR('',#12415,10.) ;
#3501 = VECTOR('',#12418,10.) ;
#3502 = VECTOR('',#12421,10.) ;
#3503 = VECTOR('',#12424,10.) ;
#3504 = VECTOR('',#12427,10.) ;
#3505 = VECTOR('',#12430,10.) ;
#3506 = VECTOR('',#12433,10.) ;
#3507 = VECTOR('',#12436,10.) ;
#3508 = VECTOR('',#12439,10.) ;
#3509 = VECTOR('',#12442,10.) ;
#3510 = VECTOR('',#12445,10.) ;
#3511 = VECTOR('',#12448,10.) ;
#3512 = VECTOR('',#12451,10.) ;
#3513 = VECTOR('',#12454,1.9) ;
#3514 = VECTOR('',#12459,10.) ;
#3515 = VECTOR('',#12462,10.) ;
#3516 = VECTOR('',#12465,10.) ;
#3517 = VECTOR('',#12468,10.) ;
#3518 = VECTOR('',#12471,10.) ;
#3519 = VECTOR('',#12474,10.) ;
#3520 = VECTOR('',#12477,10.) ;
#3521 = VECTOR('',#12480,10.) ;
#3522 = VECTOR('',#12483,10.) ;
#3523 = VECTOR('',#12486,10.) ;
#3524 = VECTOR('',#12489,10.) ;
#3525 = VECTOR('',#12492,10.) ;
#3526 = VECTOR('',#12495,10.) ;
#3527 = VECTOR('',#12498,10.) ;
#3528 = VECTOR('',#12501,10.) ;
#3529 = VECTOR('',#12504,10.) ;
#3530 = VECTOR('',#12507,10.) ;
#3531 = VECTOR('',#12510,10.) ;
#3532 = VECTOR('',#12513,10.) ;
#3533 = VECTOR('',#12516,10.) ;
#3534 = VECTOR('',#12519,10.) ;
#3535 = VECTOR('',#12522,10.) ;
#3536 = VECTOR('',#12525,10.) ;
#3537 = VECTOR('',#12528,10.) ;
#3538 = VECTOR('',#12531,10.) ;
#3539 = VECTOR('',#12534,10.) ;
#3540 = VECTOR('',#12537,10.) ;
#3541 = VECTOR('',#12540,10.) ;
#3542 = VECTOR('',#12543,10.) ;
#3543 = VECTOR('',#12546,10.) ;
#3544 = VECTOR('',#12549,10.) ;
#3545 = VECTOR('',#12552,10.) ;
#3546 = VECTOR('',#12555,10.) ;
#3547 = VECTOR('',#12560,10.) ;
#3548 = VECTOR('',#12561,10.) ;
#3549 = VECTOR('',#12564,10.) ;
#3550 = VECTOR('',#12571,1.75) ;
#3551 = VECTOR('',#12574,10.) ;
#3552 = VECTOR('',#12575,10.) ;
#3553 = VECTOR('',#12578,10.) ;
#3554 = VECTOR('',#12583,10.) ;
#3555 = VECTOR('',#12584,10.) ;
#3556 = VECTOR('',#12587,10.) ;
#3557 = VECTOR('',#12592,10.) ;
#3558 = VECTOR('',#12593,10.) ;
#3559 = VECTOR('',#12596,10.) ;
#3560 = VECTOR('',#12601,10.) ;
#3561 = VECTOR('',#12602,10.) ;
#3562 = VECTOR('',#12605,10.) ;
#3563 = VECTOR('',#12610,10.) ;
#3564 = VECTOR('',#12611,10.) ;
#3565 = VECTOR('',#12614,10.) ;
#3566 = VECTOR('',#12619,10.) ;
#3567 = VECTOR('',#12620,10.) ;
#3568 = VECTOR('',#12623,10.) ;
#3569 = VECTOR('',#12628,10.) ;
#3570 = VECTOR('',#12629,10.) ;
#3571 = VECTOR('',#12632,10.) ;
#3572 = VECTOR('',#12637,10.) ;
#3573 = VECTOR('',#12638,10.) ;
#3574 = VECTOR('',#12641,10.) ;
#3575 = VECTOR('',#12646,10.) ;
#3576 = VECTOR('',#12647,10.) ;
#3577 = VECTOR('',#12650,10.) ;
#3578 = VECTOR('',#12655,10.) ;
#3579 = VECTOR('',#12656,10.) ;
#3580 = VECTOR('',#12659,10.) ;
#3581 = VECTOR('',#12664,10.) ;
#3582 = VECTOR('',#12665,10.) ;
#3583 = VECTOR('',#12668,10.) ;
#3584 = VECTOR('',#12673,10.) ;
#3585 = VECTOR('',#12674,10.) ;
#3586 = VECTOR('',#12677,10.) ;
#3587 = VECTOR('',#12682,10.) ;
#3588 = VECTOR('',#12683,10.) ;
#3589 = VECTOR('',#12686,10.) ;
#3590 = VECTOR('',#12691,10.) ;
#3591 = VECTOR('',#12692,10.) ;
#3592 = VECTOR('',#12695,10.) ;
#3593 = VECTOR('',#12700,10.) ;
#3594 = VECTOR('',#12701,10.) ;
#3595 = VECTOR('',#12704,10.) ;
#3596 = VECTOR('',#12709,10.) ;
#3597 = VECTOR('',#12710,10.) ;
#3598 = VECTOR('',#12713,10.) ;
#3599 = VECTOR('',#12718,10.) ;
#3600 = VECTOR('',#12719,10.) ;
#3601 = VECTOR('',#12722,10.) ;
#3602 = VECTOR('',#12727,10.) ;
#3603 = VECTOR('',#12728,10.) ;
#3604 = VECTOR('',#12731,10.) ;
#3605 = VECTOR('',#12736,10.) ;
#3606 = VECTOR('',#12737,10.) ;
#3607 = VECTOR('',#12740,10.) ;
#3608 = VECTOR('',#12745,10.) ;
#3609 = VECTOR('',#12746,10.) ;
#3610 = VECTOR('',#12749,10.) ;
#3611 = VECTOR('',#12754,10.) ;
#3612 = VECTOR('',#12755,10.) ;
#3613 = VECTOR('',#12758,10.) ;
#3614 = VECTOR('',#12763,10.) ;
#3615 = VECTOR('',#12764,10.) ;
#3616 = VECTOR('',#12767,10.) ;
#3617 = VECTOR('',#12772,10.) ;
#3618 = VECTOR('',#12773,10.) ;
#3619 = VECTOR('',#12776,10.) ;
#3620 = VECTOR('',#12781,10.) ;
#3621 = VECTOR('',#12782,10.) ;
#3622 = VECTOR('',#12785,10.) ;
#3623 = VECTOR('',#12790,10.) ;
#3624 = VECTOR('',#12791,10.) ;
#3625 = VECTOR('',#12794,10.) ;
#3626 = VECTOR('',#12799,10.) ;
#3627 = VECTOR('',#12800,10.) ;
#3628 = VECTOR('',#12803,10.) ;
#3629 = VECTOR('',#12808,10.) ;
#3630 = VECTOR('',#12809,10.) ;
#3631 = VECTOR('',#12812,10.) ;
#3632 = VECTOR('',#12817,10.) ;
#3633 = VECTOR('',#12818,10.) ;
#3634 = VECTOR('',#12821,10.) ;
#3635 = VECTOR('',#12826,10.) ;
#3636 = VECTOR('',#12827,10.) ;
#3637 = VECTOR('',#12830,10.) ;
#3638 = VECTOR('',#12835,10.) ;
#3639 = VECTOR('',#12836,10.) ;
#3640 = VECTOR('',#12839,10.) ;
#3641 = VECTOR('',#12844,10.) ;
#3642 = VECTOR('',#12845,10.) ;
#3643 = VECTOR('',#12848,10.) ;
#3644 = VECTOR('',#12853,10.) ;
#3645 = VECTOR('',#12854,10.) ;
#3646 = VECTOR('',#12857,10.) ;
#3647 = VECTOR('',#12862,10.) ;
#3648 = VECTOR('',#12863,10.) ;
#3649 = VECTOR('',#12866,10.) ;
#3650 = VECTOR('',#12871,10.) ;
#3651 = VECTOR('',#12872,10.) ;
#3652 = VECTOR('',#12875,10.) ;
#3653 = VECTOR('',#12888,0.916025403784442) ;
#3654 = VECTOR('',#12903,10.) ;
#3655 = VECTOR('',#12904,10.) ;
#3656 = VECTOR('',#12909,10.) ;
#3657 = VECTOR('',#12910,10.) ;
#3658 = VECTOR('',#12915,10.) ;
#3659 = VECTOR('',#12918,10.) ;
#3660 = VECTOR('',#12921,10.) ;
#3661 = VECTOR('',#12922,10.) ;
#3662 = VECTOR('',#12927,10.) ;
#3663 = VECTOR('',#12930,10.) ;
#3664 = VECTOR('',#12933,10.) ;
#3665 = VECTOR('',#12936,10.) ;
#3666 = VECTOR('',#12939,10.) ;
#3667 = VECTOR('',#12940,10.) ;
#3668 = VECTOR('',#12941,10.) ;
#3669 = VECTOR('',#12942,10.) ;
#3670 = VECTOR('',#12945,10.) ;
#3671 = VECTOR('',#12946,10.) ;
#3672 = VECTOR('',#12947,10.) ;
#3673 = VECTOR('',#12950,10.) ;
#3674 = VECTOR('',#12951,10.) ;
#3675 = VECTOR('',#12952,10.) ;
#3676 = VECTOR('',#12959,10.) ;
#3677 = VECTOR('',#12964,10.) ;
#3678 = VECTOR('',#12967,10.) ;
#3679 = VECTOR('',#12970,10.) ;
#3680 = VECTOR('',#12987,10.) ;
#3681 = VECTOR('',#12992,10.) ;
#3682 = VECTOR('',#12997,0.866025403784434) ;
#3683 = VECTOR('',#13000,10.) ;
#3684 = VECTOR('',#13003,10.) ;
#3685 = VECTOR('',#13012,1.15) ;
#3686 = VECTOR('',#13019,1.15) ;
#3687 = VECTOR('',#13026,10.) ;
#3688 = VECTOR('',#13027,10.) ;
#3689 = VECTOR('',#13028,10.) ;
#3690 = VECTOR('',#13029,10.) ;
#3691 = VECTOR('',#13030,10.) ;
#3692 = VECTOR('',#13035,2.04999999999999) ;
#3693 = VECTOR('',#13040,10.) ;
#3694 = VECTOR('',#13041,10.) ;
#3695 = VECTOR('',#13042,10.) ;
#3696 = VECTOR('',#13049,10.) ;
#3697 = VECTOR('',#13052,10.) ;
#3698 = VECTOR('',#13053,10.) ;
#3699 = VECTOR('',#13056,10.) ;
#3700 = VECTOR('',#13057,10.) ;
#3701 = VECTOR('',#13058,10.) ;
#3702 = VECTOR('',#13067,10.) ;
#3703 = VECTOR('',#13072,10.) ;
#3704 = VECTOR('',#13073,10.) ;
#3705 = VECTOR('',#13074,10.) ;
#3706 = VECTOR('',#13075,10.) ;
#3707 = VECTOR('',#13078,10.) ;
#3708 = VECTOR('',#13079,10.) ;
#3709 = VECTOR('',#13086,2.04999999999999) ;
#3710 = VECTOR('',#13089,10.) ;
#3711 = VECTOR('',#13090,10.) ;
#3712 = VECTOR('',#13091,10.) ;
#3713 = VECTOR('',#13096,10.) ;
#3714 = VECTOR('',#13099,10.) ;
#3715 = VECTOR('',#13100,10.) ;
#3716 = VECTOR('',#13105,10.) ;
#3717 = VECTOR('',#13112,4.4) ;
#3718 = VECTOR('',#13119,1.49999999999999) ;
#3719 = VECTOR('',#13124,10.) ;
#3720 = VECTOR('',#13125,10.) ;
#3721 = VECTOR('',#13126,10.) ;
#3722 = VECTOR('',#13127,10.) ;
#3723 = VECTOR('',#13130,10.) ;
#3724 = VECTOR('',#13131,10.) ;
#3725 = VECTOR('',#13132,10.) ;
#3726 = VECTOR('',#13135,10.) ;
#3727 = VECTOR('',#13136,10.) ;
#3728 = VECTOR('',#13137,10.) ;
#3729 = VECTOR('',#13140,10.) ;
#3730 = VECTOR('',#13141,10.) ;
#3731 = VECTOR('',#13152,1.15) ;
#3732 = VECTOR('',#13159,1.15) ;
#3733 = VECTOR('',#13164,10.) ;
#3734 = VECTOR('',#13165,10.) ;
#3735 = VECTOR('',#13168,10.) ;
#3736 = VECTOR('',#13173,10.) ;
#3737 = VECTOR('',#13174,10.) ;
#3738 = VECTOR('',#13175,10.) ;
#3739 = VECTOR('',#13178,2.05) ;
#3740 = VECTOR('',#13183,10.) ;
#3741 = VECTOR('',#13184,10.) ;
#3742 = VECTOR('',#13185,10.) ;
#3743 = VECTOR('',#13192,10.) ;
#3744 = VECTOR('',#13195,10.) ;
#3745 = VECTOR('',#13196,10.) ;
#3746 = VECTOR('',#13199,10.) ;
#3747 = VECTOR('',#13204,10.) ;
#3748 = VECTOR('',#13205,10.) ;
#3749 = VECTOR('',#13206,10.) ;
#3750 = VECTOR('',#13209,2.05) ;
#3751 = VECTOR('',#13214,10.) ;
#3752 = VECTOR('',#13215,10.) ;
#3753 = VECTOR('',#13216,10.) ;
#3754 = VECTOR('',#13223,10.) ;
#3755 = VECTOR('',#13226,10.) ;
#3756 = VECTOR('',#13227,10.) ;
#3757 = VECTOR('',#13228,10.) ;
#3758 = VECTOR('',#13229,10.) ;
#3759 = VECTOR('',#13232,10.) ;
#3760 = VECTOR('',#13233,10.) ;
#3761 = VECTOR('',#13234,10.) ;
#3762 = VECTOR('',#13237,10.) ;
#3763 = VECTOR('',#13238,10.) ;
#3764 = VECTOR('',#13239,10.) ;
#3765 = VECTOR('',#13242,10.) ;
#3766 = VECTOR('',#13243,10.) ;
#3767 = VECTOR('',#13260,6.00000000000001) ;
#3768 = VECTOR('',#13269,10.35) ;
#3769 = VECTOR('',#13274,11.35) ;
#3770 = VECTOR('',#13279,11.65) ;
#3771 = VECTOR('',#13284,11.35) ;
#3772 = VECTOR('',#13289,10.35) ;
#3773 = VECTOR('',#13298,6.00000000000001) ;
#3774 = VECTOR('',#13305,2.04999999999999) ;
#3775 = CIRCLE('',#9750,1.20000000000001) ;
#3776 = CIRCLE('',#9751,1.05) ;
#3777 = CIRCLE('',#9753,1.2) ;
#3778 = CIRCLE('',#9755,1.05) ;
#3779 = CIRCLE('',#9757,1.20000000000001) ;
#3780 = CIRCLE('',#9758,1.05) ;
#3781 = CIRCLE('',#9760,1.2) ;
#3782 = CIRCLE('',#9762,1.05) ;
#3783 = CIRCLE('',#9764,1.20000000000001) ;
#3784 = CIRCLE('',#9765,1.05) ;
#3785 = CIRCLE('',#9767,1.2) ;
#3786 = CIRCLE('',#9769,1.05) ;
#3787 = CIRCLE('',#9771,1.20000000000001) ;
#3788 = CIRCLE('',#9772,1.05) ;
#3789 = CIRCLE('',#9774,1.2) ;
#3790 = CIRCLE('',#9776,1.05) ;
#3791 = CIRCLE('',#9778,1.05) ;
#3792 = CIRCLE('',#9780,1.05) ;
#3793 = CIRCLE('',#9781,1.05) ;
#3794 = CIRCLE('',#9783,1.05) ;
#3795 = CIRCLE('',#9785,1.05) ;
#3796 = CIRCLE('',#9786,1.05) ;
#3797 = CIRCLE('',#9788,1.05) ;
#3798 = CIRCLE('',#9790,1.05) ;
#3799 = CIRCLE('',#9792,1.05) ;
#3800 = CIRCLE('',#9794,1.05) ;
#3801 = CIRCLE('',#9801,2.05) ;
#3802 = CIRCLE('',#9802,2.05) ;
#3803 = CIRCLE('',#9806,2.05) ;
#3804 = CIRCLE('',#9807,2.05) ;
#3805 = CIRCLE('',#9811,2.95) ;
#3806 = CIRCLE('',#9812,2.95) ;
#3807 = CIRCLE('',#9816,2.95) ;
#3808 = CIRCLE('',#9817,2.95) ;
#3809 = CIRCLE('',#9820,2.05) ;
#3810 = CIRCLE('',#9821,2.05) ;
#3811 = CIRCLE('',#9823,2.05) ;
#3812 = CIRCLE('',#9824,2.05) ;
#3813 = CIRCLE('',#9826,2.05) ;
#3814 = CIRCLE('',#9827,2.05) ;
#3815 = CIRCLE('',#9829,2.05) ;
#3816 = CIRCLE('',#9830,2.05) ;
#3817 = CIRCLE('',#9833,3.50000000000001) ;
#3818 = CIRCLE('',#9836,3.50000000000001) ;
#3819 = CIRCLE('',#9843,3.99999999999999) ;
#3820 = CIRCLE('',#9844,3.99999999999999) ;
#3821 = CIRCLE('',#9845,3.99999999999999) ;
#3822 = CIRCLE('',#9846,3.99999999999999) ;
#3823 = CIRCLE('',#9847,3.99999999999999) ;
#3824 = CIRCLE('',#9848,3.99999999999999) ;
#3825 = CIRCLE('',#9854,3.99999999999999) ;
#3826 = CIRCLE('',#9858,3.50000000000001) ;
#3827 = CIRCLE('',#9864,3.99999999999999) ;
#3828 = CIRCLE('',#9865,3.99999999999999) ;
#3829 = CIRCLE('',#9866,3.99999999999999) ;
#3830 = CIRCLE('',#9867,3.99999999999999) ;
#3831 = CIRCLE('',#9868,3.99999999999999) ;
#3832 = CIRCLE('',#9875,3.50000000000001) ;
#3833 = CIRCLE('',#9907,2.05) ;
#3834 = CIRCLE('',#9908,2.05) ;
#3835 = CIRCLE('',#9910,2.05) ;
#3836 = CIRCLE('',#9911,2.05) ;
#3837 = CIRCLE('',#9918,5.00000000000001) ;
#3838 = CIRCLE('',#9919,5.00000000000001) ;
#3839 = CIRCLE('',#9921,5.00000000000001) ;
#3840 = CIRCLE('',#9922,5.00000000000001) ;
#3841 = CIRCLE('',#9924,6.00000000000001) ;
#3842 = CIRCLE('',#9925,6.00000000000001) ;
#3843 = CIRCLE('',#9926,6.00000000000001) ;
#3844 = CIRCLE('',#9927,6.00000000000001) ;
#3845 = CIRCLE('',#9928,5.00000000000001) ;
#3846 = CIRCLE('',#9929,5.00000000000001) ;
#3847 = CIRCLE('',#9930,5.00000000000001) ;
#3848 = CIRCLE('',#9931,5.00000000000001) ;
#3849 = CIRCLE('',#9938,5.00000000000001) ;
#3850 = CIRCLE('',#9940,5.00000000000001) ;
#3851 = CIRCLE('',#9942,0.499999999999989) ;
#3852 = CIRCLE('',#9943,0.499999999999998) ;
#3853 = CIRCLE('',#9945,0.500000000000007) ;
#3854 = CIRCLE('',#9946,5.50000000000001) ;
#3855 = CIRCLE('',#9947,6.00000000000002) ;
#3856 = CIRCLE('',#9949,0.499999999999998) ;
#3857 = CIRCLE('',#9951,0.499999999999998) ;
#3858 = CIRCLE('',#9952,5.50000000000001) ;
#3859 = CIRCLE('',#9953,6.00000000000002) ;
#3860 = CIRCLE('',#9955,0.499999999999998) ;
#3861 = CIRCLE('',#9957,0.500000000000007) ;
#3862 = CIRCLE('',#9958,5.50000000000001) ;
#3863 = CIRCLE('',#9959,6.00000000000002) ;
#3864 = CIRCLE('',#9961,0.499999999999998) ;
#3865 = CIRCLE('',#9963,5.50000000000001) ;
#3866 = CIRCLE('',#9964,6.00000000000002) ;
#3867 = CIRCLE('',#9972,5.00000000000001) ;
#3868 = CIRCLE('',#9977,5.00000000000001) ;
#3869 = CIRCLE('',#9985,2.5) ;
#3870 = CIRCLE('',#9986,2.5) ;
#3871 = CIRCLE('',#9988,1.5) ;
#3872 = CIRCLE('',#9989,1.5) ;
#3873 = CIRCLE('',#9991,2.05) ;
#3874 = CIRCLE('',#9992,2.05) ;
#3875 = CIRCLE('',#9994,2.05) ;
#3876 = CIRCLE('',#9995,2.05) ;
#3877 = CIRCLE('',#9998,3.8) ;
#3878 = CIRCLE('',#9999,3.8) ;
#3879 = CIRCLE('',#10002,3.8) ;
#3880 = CIRCLE('',#10003,3.8) ;
#3881 = CIRCLE('',#10007,1.5) ;
#3882 = CIRCLE('',#10008,1.5) ;
#3883 = CIRCLE('',#10010,2.05) ;
#3884 = CIRCLE('',#10011,2.05) ;
#3885 = CIRCLE('',#10013,2.05) ;
#3886 = CIRCLE('',#10014,2.05) ;
#3887 = CIRCLE('',#10017,3.8) ;
#3888 = CIRCLE('',#10018,3.8) ;
#3889 = CIRCLE('',#10021,3.8) ;
#3890 = CIRCLE('',#10022,3.8) ;
#3891 = CIRCLE('',#10027,2.5) ;
#3892 = CIRCLE('',#10028,2.5) ;
#3893 = CIRCLE('',#10030,2.5) ;
#3894 = CIRCLE('',#10031,2.5) ;
#3895 = CIRCLE('',#10033,2.05) ;
#3896 = CIRCLE('',#10034,2.05) ;
#3897 = CIRCLE('',#10036,1.5) ;
#3898 = CIRCLE('',#10037,1.5) ;
#3899 = CIRCLE('',#10039,2.05) ;
#3900 = CIRCLE('',#10040,2.05) ;
#3901 = CIRCLE('',#10043,3.8) ;
#3902 = CIRCLE('',#10044,3.8) ;
#3903 = CIRCLE('',#10047,3.8) ;
#3904 = CIRCLE('',#10048,3.8) ;
#3905 = CIRCLE('',#10052,1.5) ;
#3906 = CIRCLE('',#10053,1.5) ;
#3907 = CIRCLE('',#10055,2.05) ;
#3908 = CIRCLE('',#10056,2.05) ;
#3909 = CIRCLE('',#10058,2.05) ;
#3910 = CIRCLE('',#10059,2.05) ;
#3911 = CIRCLE('',#10062,3.8) ;
#3912 = CIRCLE('',#10063,3.8) ;
#3913 = CIRCLE('',#10066,3.8) ;
#3914 = CIRCLE('',#10067,3.8) ;
#3915 = CIRCLE('',#10072,3.) ;
#3916 = CIRCLE('',#10074,3.) ;
#3917 = CIRCLE('',#10075,3.) ;
#3918 = CIRCLE('',#10077,2.05) ;
#3919 = CIRCLE('',#10078,2.05) ;
#3920 = CIRCLE('',#10080,4.6) ;
#3921 = CIRCLE('',#10082,4.6) ;
#3922 = CIRCLE('',#10084,2.1) ;
#3923 = CIRCLE('',#10086,2.09999999999999) ;
#3924 = CIRCLE('',#10088,4.99999999999999) ;
#3925 = CIRCLE('',#10090,5.) ;
#3926 = CIRCLE('',#10092,1.99999999999999) ;
#3927 = CIRCLE('',#10095,3.) ;
#3928 = CIRCLE('',#10100,3.5) ;
#3929 = CIRCLE('',#10101,3.5) ;
#3930 = CIRCLE('',#10103,2.55) ;
#3931 = CIRCLE('',#10104,2.55) ;
#3932 = CIRCLE('',#10106,3.5) ;
#3933 = CIRCLE('',#10107,3.5) ;
#3934 = CIRCLE('',#10111,2.) ;
#3935 = CIRCLE('',#10112,2.) ;
#3936 = CIRCLE('',#10114,2.) ;
#3937 = CIRCLE('',#10116,2.) ;
#3938 = CIRCLE('',#10118,4.50000000000001) ;
#3939 = CIRCLE('',#10120,4.50000000000001) ;
#3940 = CIRCLE('',#10124,2.05) ;
#3941 = CIRCLE('',#10125,2.05) ;
#3942 = CIRCLE('',#10130,5.) ;
#3943 = CIRCLE('',#10132,5.) ;
#3944 = CIRCLE('',#10137,4.49999999999999) ;
#3945 = CIRCLE('',#10139,5.) ;
#3946 = CIRCLE('',#10140,5.) ;
#3947 = CIRCLE('',#10142,5.) ;
#3948 = CIRCLE('',#10144,5.) ;
#3949 = CIRCLE('',#10145,5.) ;
#3950 = CIRCLE('',#10159,2.19999999999999) ;
#3951 = CIRCLE('',#10160,2.2) ;
#3952 = CIRCLE('',#10161,2.05) ;
#3953 = CIRCLE('',#10164,2.05) ;
#3954 = CIRCLE('',#10166,2.2) ;
#3955 = CIRCLE('',#10169,2.19999999999999) ;
#3956 = CIRCLE('',#10175,2.05) ;
#3957 = CIRCLE('',#10176,2.05) ;
#3958 = CIRCLE('',#10178,2.85) ;
#3959 = CIRCLE('',#10185,2.85) ;
#3960 = CIRCLE('',#10187,2.85) ;
#3961 = CIRCLE('',#10188,2.85) ;
#3962 = CIRCLE('',#10189,2.85) ;
#3963 = CIRCLE('',#10191,7.15) ;
#3964 = CIRCLE('',#10192,2.85) ;
#3965 = CIRCLE('',#10193,2.85) ;
#3966 = CIRCLE('',#10195,2.85) ;
#3967 = CIRCLE('',#10196,2.85) ;
#3968 = CIRCLE('',#10198,7.15000000000003) ;
#3969 = CIRCLE('',#10199,2.85) ;
#3970 = CIRCLE('',#10200,2.85) ;
#3971 = CIRCLE('',#10202,2.85) ;
#3972 = CIRCLE('',#10207,2.05) ;
#3973 = CIRCLE('',#10208,2.05) ;
#3974 = CIRCLE('',#10211,2.2) ;
#3975 = CIRCLE('',#10212,2.2) ;
#3976 = CIRCLE('',#10215,2.20000000000001) ;
#3977 = CIRCLE('',#10216,2.20000000000001) ;
#3978 = CIRCLE('',#10221,2.79999999999999) ;
#3979 = CIRCLE('',#10223,3.) ;
#3980 = CIRCLE('',#10225,3.) ;
#3981 = CIRCLE('',#10227,2.) ;
#3982 = CIRCLE('',#10229,2.) ;
#3983 = CIRCLE('',#10231,1.59999999999999) ;
#3984 = CIRCLE('',#10233,1.59999999999999) ;
#3985 = CIRCLE('',#10235,2.) ;
#3986 = CIRCLE('',#10237,2.) ;
#3987 = CIRCLE('',#10239,1.75) ;
#3988 = CIRCLE('',#10247,1.59999999999999) ;
#3989 = CIRCLE('',#10248,1.59999999999999) ;
#3990 = CIRCLE('',#10250,3.65) ;
#3991 = CIRCLE('',#10252,3.65) ;
#3992 = CIRCLE('',#10256,3.70000000000001) ;
#3993 = CIRCLE('',#10258,4.) ;
#3994 = CIRCLE('',#10260,4.) ;
#3995 = CIRCLE('',#10262,3.70000000000001) ;
#3996 = CIRCLE('',#10264,1.5) ;
#3997 = CIRCLE('',#10266,1.5) ;
#3998 = CIRCLE('',#10268,1.3) ;
#3999 = CIRCLE('',#10272,0.96675) ;
#4000 = CIRCLE('',#10287,0.739000000000001) ;
#4001 = CIRCLE('',#10302,0.96675) ;
#4002 = CIRCLE('',#10303,0.96675) ;
#4003 = CIRCLE('',#10305,0.96675) ;
#4004 = CIRCLE('',#10306,0.739000000000001) ;
#4005 = CIRCLE('',#10307,0.96675) ;
#4006 = CIRCLE('',#10310,0.1) ;
#4007 = CIRCLE('',#10311,1.06675) ;
#4008 = CIRCLE('',#10313,0.96675) ;
#4009 = CIRCLE('',#10315,1.69999999999999) ;
#4010 = CIRCLE('',#10317,0.616749999999999) ;
#4011 = CIRCLE('',#10320,1.9) ;
#4012 = CIRCLE('',#10324,1.9) ;
#4013 = CIRCLE('',#10325,1.9) ;
#4014 = CIRCLE('',#10326,1.9) ;
#4015 = CIRCLE('',#10327,1.9) ;
#4016 = CIRCLE('',#10328,1.9) ;
#4017 = CIRCLE('',#10329,1.9) ;
#4018 = CIRCLE('',#10330,1.9) ;
#4019 = CIRCLE('',#10331,1.9) ;
#4020 = CIRCLE('',#10332,1.9) ;
#4021 = CIRCLE('',#10333,1.9) ;
#4022 = CIRCLE('',#10334,1.9) ;
#4023 = CIRCLE('',#10335,1.9) ;
#4024 = CIRCLE('',#10336,1.9) ;
#4025 = CIRCLE('',#10337,1.9) ;
#4026 = CIRCLE('',#10338,1.9) ;
#4027 = CIRCLE('',#10339,1.9) ;
#4028 = CIRCLE('',#10340,1.9) ;
#4029 = CIRCLE('',#10341,1.9) ;
#4030 = CIRCLE('',#10342,1.9) ;
#4031 = CIRCLE('',#10343,1.9) ;
#4032 = CIRCLE('',#10344,1.9) ;
#4033 = CIRCLE('',#10345,1.9) ;
#4034 = CIRCLE('',#10346,1.9) ;
#4035 = CIRCLE('',#10347,1.9) ;
#4036 = CIRCLE('',#10348,1.9) ;
#4037 = CIRCLE('',#10349,1.9) ;
#4038 = CIRCLE('',#10350,1.9) ;
#4039 = CIRCLE('',#10351,1.9) ;
#4040 = CIRCLE('',#10352,1.9) ;
#4041 = CIRCLE('',#10353,1.9) ;
#4042 = CIRCLE('',#10354,1.9) ;
#4043 = CIRCLE('',#10355,1.9) ;
#4044 = CIRCLE('',#10356,1.9) ;
#4045 = CIRCLE('',#10357,1.9) ;
#4046 = CIRCLE('',#10358,1.9) ;
#4047 = CIRCLE('',#10359,1.9) ;
#4048 = CIRCLE('',#10360,1.9) ;
#4049 = CIRCLE('',#10361,1.9) ;
#4050 = CIRCLE('',#10362,1.9) ;
#4051 = CIRCLE('',#10363,1.9) ;
#4052 = CIRCLE('',#10364,1.9) ;
#4053 = CIRCLE('',#10365,1.9) ;
#4054 = CIRCLE('',#10366,1.9) ;
#4055 = CIRCLE('',#10367,1.9) ;
#4056 = CIRCLE('',#10368,1.9) ;
#4057 = CIRCLE('',#10369,1.9) ;
#4058 = CIRCLE('',#10370,1.9) ;
#4059 = CIRCLE('',#10371,1.9) ;
#4060 = CIRCLE('',#10372,1.9) ;
#4061 = CIRCLE('',#10373,1.9) ;
#4062 = CIRCLE('',#10374,1.9) ;
#4063 = CIRCLE('',#10375,1.9) ;
#4064 = CIRCLE('',#10376,1.9) ;
#4065 = CIRCLE('',#10377,1.9) ;
#4066 = CIRCLE('',#10378,1.9) ;
#4067 = CIRCLE('',#10379,1.9) ;
#4068 = CIRCLE('',#10380,1.9) ;
#4069 = CIRCLE('',#10381,1.9) ;
#4070 = CIRCLE('',#10382,1.9) ;
#4071 = CIRCLE('',#10383,1.9) ;
#4072 = CIRCLE('',#10384,1.9) ;
#4073 = CIRCLE('',#10385,1.9) ;
#4074 = CIRCLE('',#10386,1.9) ;
#4075 = CIRCLE('',#10387,1.9) ;
#4076 = CIRCLE('',#10388,1.9) ;
#4077 = CIRCLE('',#10389,1.9) ;
#4078 = CIRCLE('',#10390,1.9) ;
#4079 = CIRCLE('',#10391,1.9) ;
#4080 = CIRCLE('',#10392,1.9) ;
#4081 = CIRCLE('',#10393,1.9) ;
#4082 = CIRCLE('',#10394,1.9) ;
#4083 = CIRCLE('',#10395,1.9) ;
#4084 = CIRCLE('',#10396,1.9) ;
#4085 = CIRCLE('',#10401,1.6) ;
#4086 = CIRCLE('',#10505,0.2) ;
#4087 = CIRCLE('',#10507,1.01602540378444) ;
#4088 = CIRCLE('',#10509,0.816025403784444) ;
#4089 = CIRCLE('',#10510,0.816025403784444) ;
#4090 = CIRCLE('',#10511,0.816025403784444) ;
#4091 = CIRCLE('',#10512,0.816025403784444) ;
#4092 = CIRCLE('',#10513,0.816025403784444) ;
#4093 = CIRCLE('',#10514,0.816025403784444) ;
#4094 = CIRCLE('',#10516,0.816025403784444) ;
#4095 = CIRCLE('',#10518,0.816025403784444) ;
#4096 = CIRCLE('',#10520,0.816025403784444) ;
#4097 = CIRCLE('',#10522,0.816025403784444) ;
#4098 = CIRCLE('',#10524,0.816025403784444) ;
#4099 = CIRCLE('',#10526,0.816025403784444) ;
#4100 = CIRCLE('',#10537,0.866025403784434) ;
#4101 = CIRCLE('',#10539,0.866025403784434) ;
#4102 = CIRCLE('',#10541,0.866025403784434) ;
#4103 = CIRCLE('',#10543,0.866025403784434) ;
#4104 = CIRCLE('',#10545,0.866025403784434) ;
#4105 = CIRCLE('',#10547,0.866025403784434) ;
#4106 = CIRCLE('',#10554,1.15) ;
#4107 = CIRCLE('',#10555,1.15) ;
#4108 = CIRCLE('',#10557,1.15) ;
#4109 = CIRCLE('',#10558,1.15) ;
#4110 = CIRCLE('',#10560,4.4) ;
#4111 = CIRCLE('',#10562,2.04999999999999) ;
#4112 = CIRCLE('',#10563,2.04999999999999) ;
#4113 = CIRCLE('',#10566,5.) ;
#4114 = CIRCLE('',#10567,5.) ;
#4115 = CIRCLE('',#10572,4.4) ;
#4116 = CIRCLE('',#10573,4.4) ;
#4117 = CIRCLE('',#10574,4.4) ;
#4118 = CIRCLE('',#10576,5.) ;
#4119 = CIRCLE('',#10577,2.04999999999999) ;
#4120 = CIRCLE('',#10579,2.04999999999999) ;
#4121 = CIRCLE('',#10582,5.) ;
#4122 = CIRCLE('',#10585,4.4) ;
#4123 = CIRCLE('',#10588,4.4) ;
#4124 = CIRCLE('',#10590,1.49999999999999) ;
#4125 = CIRCLE('',#10592,1.49999999999999) ;
#4126 = CIRCLE('',#10601,1.15) ;
#4127 = CIRCLE('',#10602,1.15) ;
#4128 = CIRCLE('',#10604,1.15) ;
#4129 = CIRCLE('',#10605,1.15) ;
#4130 = CIRCLE('',#10607,4.99999999999999) ;
#4131 = CIRCLE('',#10608,2.05) ;
#4132 = CIRCLE('',#10611,2.05) ;
#4133 = CIRCLE('',#10614,4.99999999999999) ;
#4134 = CIRCLE('',#10617,4.99999999999999) ;
#4135 = CIRCLE('',#10618,2.05) ;
#4136 = CIRCLE('',#10621,2.05) ;
#4137 = CIRCLE('',#10624,4.99999999999999) ;
#4138 = CIRCLE('',#10634,6.00000000000001) ;
#4139 = CIRCLE('',#10635,2.04999999999999) ;
#4140 = CIRCLE('',#10637,6.00000000000001) ;
#4141 = CIRCLE('',#10639,9.65000000000001) ;
#4142 = CIRCLE('',#10641,11.05) ;
#4143 = CIRCLE('',#10643,11.65) ;
#4144 = CIRCLE('',#10645,11.65) ;
#4145 = CIRCLE('',#10647,11.05) ;
#4146 = CIRCLE('',#10649,9.65000000000001) ;
#4147 = CIRCLE('',#10651,6.00000000000001) ;
#4148 = CIRCLE('',#10653,6.00000000000001) ;
#4149 = CIRCLE('',#10655,2.04999999999999) ;
#4150 = VERTEX_POINT('',#13425) ;
#4151 = VERTEX_POINT('',#13427) ;
#4152 = VERTEX_POINT('',#13431) ;
#4153 = VERTEX_POINT('',#13432) ;
#4154 = VERTEX_POINT('',#13434) ;
#4155 = VERTEX_POINT('',#13436) ;
#4156 = VERTEX_POINT('',#13439) ;
#4157 = VERTEX_POINT('',#13442) ;
#4158 = VERTEX_POINT('',#13446) ;
#4159 = VERTEX_POINT('',#13448) ;
#4160 = VERTEX_POINT('',#13452) ;
#4161 = VERTEX_POINT('',#13453) ;
#4162 = VERTEX_POINT('',#13455) ;
#4163 = VERTEX_POINT('',#13457) ;
#4164 = VERTEX_POINT('',#13460) ;
#4165 = VERTEX_POINT('',#13463) ;
#4166 = VERTEX_POINT('',#13467) ;
#4167 = VERTEX_POINT('',#13469) ;
#4168 = VERTEX_POINT('',#13473) ;
#4169 = VERTEX_POINT('',#13474) ;
#4170 = VERTEX_POINT('',#13476) ;
#4171 = VERTEX_POINT('',#13478) ;
#4172 = VERTEX_POINT('',#13481) ;
#4173 = VERTEX_POINT('',#13484) ;
#4174 = VERTEX_POINT('',#13488) ;
#4175 = VERTEX_POINT('',#13490) ;
#4176 = VERTEX_POINT('',#13494) ;
#4177 = VERTEX_POINT('',#13495) ;
#4178 = VERTEX_POINT('',#13497) ;
#4179 = VERTEX_POINT('',#13499) ;
#4180 = VERTEX_POINT('',#13502) ;
#4181 = VERTEX_POINT('',#13505) ;
#4182 = VERTEX_POINT('',#13509) ;
#4183 = VERTEX_POINT('',#13513) ;
#4184 = VERTEX_POINT('',#13515) ;
#4185 = VERTEX_POINT('',#13517) ;
#4186 = VERTEX_POINT('',#13555) ;
#4187 = VERTEX_POINT('',#13559) ;
#4188 = VERTEX_POINT('',#13561) ;
#4189 = VERTEX_POINT('',#13563) ;
#4190 = VERTEX_POINT('',#13601) ;
#4191 = VERTEX_POINT('',#13605) ;
#4192 = VERTEX_POINT('',#13609) ;
#4193 = VERTEX_POINT('',#13613) ;
#4194 = VERTEX_POINT('',#13617) ;
#4195 = VERTEX_POINT('',#13620) ;
#4196 = VERTEX_POINT('',#13623) ;
#4197 = VERTEX_POINT('',#13626) ;
#4198 = VERTEX_POINT('',#13637) ;
#4199 = VERTEX_POINT('',#13639) ;
#4200 = VERTEX_POINT('',#13643) ;
#4201 = VERTEX_POINT('',#13654) ;
#4202 = VERTEX_POINT('',#13656) ;
#4203 = VERTEX_POINT('',#13660) ;
#4204 = VERTEX_POINT('',#13663) ;
#4205 = VERTEX_POINT('',#13664) ;
#4206 = VERTEX_POINT('',#13701) ;
#4207 = VERTEX_POINT('',#13703) ;
#4208 = VERTEX_POINT('',#13741) ;
#4209 = VERTEX_POINT('',#13743) ;
#4210 = VERTEX_POINT('',#13748) ;
#4211 = VERTEX_POINT('',#13749) ;
#4212 = VERTEX_POINT('',#13786) ;
#4213 = VERTEX_POINT('',#13788) ;
#4214 = VERTEX_POINT('',#13826) ;
#4215 = VERTEX_POINT('',#13828) ;
#4216 = VERTEX_POINT('',#13833) ;
#4217 = VERTEX_POINT('',#13835) ;
#4218 = VERTEX_POINT('',#13839) ;
#4219 = VERTEX_POINT('',#13841) ;
#4220 = VERTEX_POINT('',#13845) ;
#4221 = VERTEX_POINT('',#13846) ;
#4222 = VERTEX_POINT('',#13848) ;
#4223 = VERTEX_POINT('',#13850) ;
#4224 = VERTEX_POINT('',#13854) ;
#4225 = VERTEX_POINT('',#13855) ;
#4226 = VERTEX_POINT('',#13857) ;
#4227 = VERTEX_POINT('',#13859) ;
#4228 = VERTEX_POINT('',#13863) ;
#4229 = VERTEX_POINT('',#13865) ;
#4230 = VERTEX_POINT('',#13869) ;
#4231 = VERTEX_POINT('',#13871) ;
#4232 = VERTEX_POINT('',#13873) ;
#4233 = VERTEX_POINT('',#13877) ;
#4234 = VERTEX_POINT('',#13879) ;
#4235 = VERTEX_POINT('',#13883) ;
#4236 = VERTEX_POINT('',#13885) ;
#4237 = VERTEX_POINT('',#13887) ;
#4238 = VERTEX_POINT('',#13891) ;
#4239 = VERTEX_POINT('',#13892) ;
#4240 = VERTEX_POINT('',#13894) ;
#4241 = VERTEX_POINT('',#13896) ;
#4242 = VERTEX_POINT('',#13900) ;
#4243 = VERTEX_POINT('',#13902) ;
#4244 = VERTEX_POINT('',#13904) ;
#4245 = VERTEX_POINT('',#13906) ;
#4246 = VERTEX_POINT('',#13910) ;
#4247 = VERTEX_POINT('',#13912) ;
#4248 = VERTEX_POINT('',#13914) ;
#4249 = VERTEX_POINT('',#13916) ;
#4250 = VERTEX_POINT('',#13918) ;
#4251 = VERTEX_POINT('',#13920) ;
#4252 = VERTEX_POINT('',#13922) ;
#4253 = VERTEX_POINT('',#13924) ;
#4254 = VERTEX_POINT('',#13926) ;
#4255 = VERTEX_POINT('',#13928) ;
#4256 = VERTEX_POINT('',#13930) ;
#4257 = VERTEX_POINT('',#13932) ;
#4258 = VERTEX_POINT('',#13935) ;
#4259 = VERTEX_POINT('',#13937) ;
#4260 = VERTEX_POINT('',#13940) ;
#4261 = VERTEX_POINT('',#13944) ;
#4262 = VERTEX_POINT('',#13946) ;
#4263 = VERTEX_POINT('',#13950) ;
#4264 = VERTEX_POINT('',#13952) ;
#4265 = VERTEX_POINT('',#13954) ;
#4266 = VERTEX_POINT('',#13958) ;
#4267 = VERTEX_POINT('',#13960) ;
#4268 = VERTEX_POINT('',#13962) ;
#4269 = VERTEX_POINT('',#13964) ;
#4270 = VERTEX_POINT('',#13968) ;
#4271 = VERTEX_POINT('',#13970) ;
#4272 = VERTEX_POINT('',#13978) ;
#4273 = VERTEX_POINT('',#13980) ;
#4274 = VERTEX_POINT('',#13982) ;
#4275 = VERTEX_POINT('',#13984) ;
#4276 = VERTEX_POINT('',#13986) ;
#4277 = VERTEX_POINT('',#13988) ;
#4278 = VERTEX_POINT('',#13990) ;
#4279 = VERTEX_POINT('',#13992) ;
#4280 = VERTEX_POINT('',#13994) ;
#4281 = VERTEX_POINT('',#13996) ;
#4282 = VERTEX_POINT('',#13999) ;
#4283 = VERTEX_POINT('',#14001) ;
#4284 = VERTEX_POINT('',#14004) ;
#4285 = VERTEX_POINT('',#14006) ;
#4286 = VERTEX_POINT('',#14014) ;
#4287 = VERTEX_POINT('',#14021) ;
#4288 = VERTEX_POINT('',#14022) ;
#4289 = VERTEX_POINT('',#14024) ;
#4290 = VERTEX_POINT('',#14026) ;
#4291 = VERTEX_POINT('',#14030) ;
#4292 = VERTEX_POINT('',#14032) ;
#4293 = VERTEX_POINT('',#14036) ;
#4294 = VERTEX_POINT('',#14040) ;
#4295 = VERTEX_POINT('',#14042) ;
#4296 = VERTEX_POINT('',#14054) ;
#4297 = VERTEX_POINT('',#14061) ;
#4298 = VERTEX_POINT('',#14062) ;
#4299 = VERTEX_POINT('',#14064) ;
#4300 = VERTEX_POINT('',#14066) ;
#4301 = VERTEX_POINT('',#14070) ;
#4302 = VERTEX_POINT('',#14072) ;
#4303 = VERTEX_POINT('',#14076) ;
#4304 = VERTEX_POINT('',#14080) ;
#4305 = VERTEX_POINT('',#14082) ;
#4306 = VERTEX_POINT('',#14086) ;
#4307 = VERTEX_POINT('',#14088) ;
#4308 = VERTEX_POINT('',#14097) ;
#4309 = VERTEX_POINT('',#14099) ;
#4310 = VERTEX_POINT('',#14106) ;
#4311 = VERTEX_POINT('',#14110) ;
#4312 = VERTEX_POINT('',#14115) ;
#4313 = VERTEX_POINT('',#14119) ;
#4314 = VERTEX_POINT('',#14123) ;
#4315 = VERTEX_POINT('',#14125) ;
#4316 = VERTEX_POINT('',#14132) ;
#4317 = VERTEX_POINT('',#14136) ;
#4318 = VERTEX_POINT('',#14149) ;
#4319 = VERTEX_POINT('',#14153) ;
#4320 = VERTEX_POINT('',#14168) ;
#4321 = VERTEX_POINT('',#14170) ;
#4322 = VERTEX_POINT('',#14174) ;
#4323 = VERTEX_POINT('',#14176) ;
#4324 = VERTEX_POINT('',#14180) ;
#4325 = VERTEX_POINT('',#14181) ;
#4326 = VERTEX_POINT('',#14183) ;
#4327 = VERTEX_POINT('',#14185) ;
#4328 = VERTEX_POINT('',#14189) ;
#4329 = VERTEX_POINT('',#14191) ;
#4330 = VERTEX_POINT('',#14193) ;
#4331 = VERTEX_POINT('',#14195) ;
#4332 = VERTEX_POINT('',#14199) ;
#4333 = VERTEX_POINT('',#14201) ;
#4334 = VERTEX_POINT('',#14207) ;
#4335 = VERTEX_POINT('',#14209) ;
#4336 = VERTEX_POINT('',#14213) ;
#4337 = VERTEX_POINT('',#14215) ;
#4338 = VERTEX_POINT('',#14219) ;
#4339 = VERTEX_POINT('',#14221) ;
#4340 = VERTEX_POINT('',#14225) ;
#4341 = VERTEX_POINT('',#14226) ;
#4342 = VERTEX_POINT('',#14228) ;
#4343 = VERTEX_POINT('',#14230) ;
#4344 = VERTEX_POINT('',#14232) ;
#4345 = VERTEX_POINT('',#14234) ;
#4346 = VERTEX_POINT('',#14236) ;
#4347 = VERTEX_POINT('',#14238) ;
#4348 = VERTEX_POINT('',#14241) ;
#4349 = VERTEX_POINT('',#14243) ;
#4350 = VERTEX_POINT('',#14245) ;
#4351 = VERTEX_POINT('',#14247) ;
#4352 = VERTEX_POINT('',#14249) ;
#4353 = VERTEX_POINT('',#14251) ;
#4354 = VERTEX_POINT('',#14253) ;
#4355 = VERTEX_POINT('',#14255) ;
#4356 = VERTEX_POINT('',#14257) ;
#4357 = VERTEX_POINT('',#14261) ;
#4358 = VERTEX_POINT('',#14262) ;
#4359 = VERTEX_POINT('',#14264) ;
#4360 = VERTEX_POINT('',#14266) ;
#4361 = VERTEX_POINT('',#14270) ;
#4362 = VERTEX_POINT('',#14272) ;
#4363 = VERTEX_POINT('',#14276) ;
#4364 = VERTEX_POINT('',#14279) ;
#4365 = VERTEX_POINT('',#14285) ;
#4366 = VERTEX_POINT('',#14289) ;
#4367 = VERTEX_POINT('',#14293) ;
#4368 = VERTEX_POINT('',#14297) ;
#4369 = VERTEX_POINT('',#14298) ;
#4370 = VERTEX_POINT('',#14300) ;
#4371 = VERTEX_POINT('',#14302) ;
#4372 = VERTEX_POINT('',#14306) ;
#4373 = VERTEX_POINT('',#14307) ;
#4374 = VERTEX_POINT('',#14312) ;
#4375 = VERTEX_POINT('',#14313) ;
#4376 = VERTEX_POINT('',#14318) ;
#4377 = VERTEX_POINT('',#14319) ;
#4378 = VERTEX_POINT('',#14324) ;
#4379 = VERTEX_POINT('',#14325) ;
#4380 = VERTEX_POINT('',#14330) ;
#4381 = VERTEX_POINT('',#14331) ;
#4382 = VERTEX_POINT('',#14336) ;
#4383 = VERTEX_POINT('',#14337) ;
#4384 = VERTEX_POINT('',#14355) ;
#4385 = VERTEX_POINT('',#14357) ;
#4386 = VERTEX_POINT('',#14361) ;
#4387 = VERTEX_POINT('',#14369) ;
#4388 = VERTEX_POINT('',#14384) ;
#4389 = VERTEX_POINT('',#14386) ;
#4390 = VERTEX_POINT('',#14390) ;
#4391 = VERTEX_POINT('',#14392) ;
#4392 = VERTEX_POINT('',#14396) ;
#4393 = VERTEX_POINT('',#14398) ;
#4394 = VERTEX_POINT('',#14402) ;
#4395 = VERTEX_POINT('',#14404) ;
#4396 = VERTEX_POINT('',#14408) ;
#4397 = VERTEX_POINT('',#14409) ;
#4398 = VERTEX_POINT('',#14411) ;
#4399 = VERTEX_POINT('',#14413) ;
#4400 = VERTEX_POINT('',#14417) ;
#4401 = VERTEX_POINT('',#14419) ;
#4402 = VERTEX_POINT('',#14423) ;
#4403 = VERTEX_POINT('',#14425) ;
#4404 = VERTEX_POINT('',#14434) ;
#4405 = VERTEX_POINT('',#14436) ;
#4406 = VERTEX_POINT('',#14440) ;
#4407 = VERTEX_POINT('',#14442) ;
#4408 = VERTEX_POINT('',#14446) ;
#4409 = VERTEX_POINT('',#14448) ;
#4410 = VERTEX_POINT('',#14452) ;
#4411 = VERTEX_POINT('',#14453) ;
#4412 = VERTEX_POINT('',#14455) ;
#4413 = VERTEX_POINT('',#14457) ;
#4414 = VERTEX_POINT('',#14461) ;
#4415 = VERTEX_POINT('',#14463) ;
#4416 = VERTEX_POINT('',#14467) ;
#4417 = VERTEX_POINT('',#14469) ;
#4418 = VERTEX_POINT('',#14479) ;
#4419 = VERTEX_POINT('',#14481) ;
#4420 = VERTEX_POINT('',#14485) ;
#4421 = VERTEX_POINT('',#14487) ;
#4422 = VERTEX_POINT('',#14491) ;
#4423 = VERTEX_POINT('',#14493) ;
#4424 = VERTEX_POINT('',#14497) ;
#4425 = VERTEX_POINT('',#14499) ;
#4426 = VERTEX_POINT('',#14503) ;
#4427 = VERTEX_POINT('',#14505) ;
#4428 = VERTEX_POINT('',#14509) ;
#4429 = VERTEX_POINT('',#14510) ;
#4430 = VERTEX_POINT('',#14512) ;
#4431 = VERTEX_POINT('',#14514) ;
#4432 = VERTEX_POINT('',#14518) ;
#4433 = VERTEX_POINT('',#14520) ;
#4434 = VERTEX_POINT('',#14524) ;
#4435 = VERTEX_POINT('',#14526) ;
#4436 = VERTEX_POINT('',#14535) ;
#4437 = VERTEX_POINT('',#14537) ;
#4438 = VERTEX_POINT('',#14541) ;
#4439 = VERTEX_POINT('',#14543) ;
#4440 = VERTEX_POINT('',#14547) ;
#4441 = VERTEX_POINT('',#14549) ;
#4442 = VERTEX_POINT('',#14553) ;
#4443 = VERTEX_POINT('',#14554) ;
#4444 = VERTEX_POINT('',#14556) ;
#4445 = VERTEX_POINT('',#14558) ;
#4446 = VERTEX_POINT('',#14562) ;
#4447 = VERTEX_POINT('',#14564) ;
#4448 = VERTEX_POINT('',#14568) ;
#4449 = VERTEX_POINT('',#14570) ;
#4450 = VERTEX_POINT('',#14580) ;
#4451 = VERTEX_POINT('',#14581) ;
#4452 = VERTEX_POINT('',#14583) ;
#4453 = VERTEX_POINT('',#14590) ;
#4454 = VERTEX_POINT('',#14591) ;
#4455 = VERTEX_POINT('',#14593) ;
#4456 = VERTEX_POINT('',#14595) ;
#4457 = VERTEX_POINT('',#14637) ;
#4458 = VERTEX_POINT('',#14639) ;
#4459 = VERTEX_POINT('',#14643) ;
#4460 = VERTEX_POINT('',#14646) ;
#4461 = VERTEX_POINT('',#14650) ;
#4462 = VERTEX_POINT('',#14653) ;
#4463 = VERTEX_POINT('',#14657) ;
#4464 = VERTEX_POINT('',#14660) ;
#4465 = VERTEX_POINT('',#14664) ;
#4466 = VERTEX_POINT('',#14678) ;
#4467 = VERTEX_POINT('',#14679) ;
#4468 = VERTEX_POINT('',#14681) ;
#4469 = VERTEX_POINT('',#14683) ;
#4470 = VERTEX_POINT('',#14692) ;
#4471 = VERTEX_POINT('',#14694) ;
#4472 = VERTEX_POINT('',#14705) ;
#4473 = VERTEX_POINT('',#14707) ;
#4474 = VERTEX_POINT('',#14712) ;
#4475 = VERTEX_POINT('',#14721) ;
#4476 = VERTEX_POINT('',#14735) ;
#4477 = VERTEX_POINT('',#14741) ;
#4478 = VERTEX_POINT('',#14745) ;
#4479 = VERTEX_POINT('',#14748) ;
#4480 = VERTEX_POINT('',#14754) ;
#4481 = VERTEX_POINT('',#14755) ;
#4482 = VERTEX_POINT('',#14757) ;
#4483 = VERTEX_POINT('',#14759) ;
#4484 = VERTEX_POINT('',#14763) ;
#4485 = VERTEX_POINT('',#14765) ;
#4486 = VERTEX_POINT('',#14767) ;
#4487 = VERTEX_POINT('',#14769) ;
#4488 = VERTEX_POINT('',#14771) ;
#4489 = VERTEX_POINT('',#14775) ;
#4490 = VERTEX_POINT('',#14777) ;
#4491 = VERTEX_POINT('',#14781) ;
#4492 = VERTEX_POINT('',#14785) ;
#4493 = VERTEX_POINT('',#14789) ;
#4494 = VERTEX_POINT('',#14790) ;
#4495 = VERTEX_POINT('',#14792) ;
#4496 = VERTEX_POINT('',#14799) ;
#4497 = VERTEX_POINT('',#14801) ;
#4498 = VERTEX_POINT('',#14804) ;
#4499 = VERTEX_POINT('',#14815) ;
#4500 = VERTEX_POINT('',#14819) ;
#4501 = VERTEX_POINT('',#14820) ;
#4502 = VERTEX_POINT('',#14824) ;
#4503 = VERTEX_POINT('',#14826) ;
#4504 = VERTEX_POINT('',#14829) ;
#4505 = VERTEX_POINT('',#14833) ;
#4506 = VERTEX_POINT('',#14835) ;
#4507 = VERTEX_POINT('',#14837) ;
#4508 = VERTEX_POINT('',#14839) ;
#4509 = VERTEX_POINT('',#14843) ;
#4510 = VERTEX_POINT('',#14844) ;
#4511 = VERTEX_POINT('',#14849) ;
#4512 = VERTEX_POINT('',#14853) ;
#4513 = VERTEX_POINT('',#14861) ;
#4514 = VERTEX_POINT('',#14862) ;
#4515 = VERTEX_POINT('',#14864) ;
#4516 = VERTEX_POINT('',#14866) ;
#4517 = VERTEX_POINT('',#14870) ;
#4518 = VERTEX_POINT('',#14872) ;
#4519 = VERTEX_POINT('',#14876) ;
#4520 = VERTEX_POINT('',#14878) ;
#4521 = VERTEX_POINT('',#14882) ;
#4522 = VERTEX_POINT('',#14883) ;
#4523 = VERTEX_POINT('',#14886) ;
#4524 = VERTEX_POINT('',#14888) ;
#4525 = VERTEX_POINT('',#14894) ;
#4526 = VERTEX_POINT('',#14896) ;
#4527 = VERTEX_POINT('',#14898) ;
#4528 = VERTEX_POINT('',#14901) ;
#4529 = VERTEX_POINT('',#14904) ;
#4530 = VERTEX_POINT('',#14908) ;
#4531 = VERTEX_POINT('',#14912) ;
#4532 = VERTEX_POINT('',#14916) ;
#4533 = VERTEX_POINT('',#14924) ;
#4534 = VERTEX_POINT('',#14925) ;
#4535 = VERTEX_POINT('',#14963) ;
#4536 = VERTEX_POINT('',#14965) ;
#4537 = VERTEX_POINT('',#15004) ;
#4538 = VERTEX_POINT('',#15005) ;
#4539 = VERTEX_POINT('',#15024) ;
#4540 = VERTEX_POINT('',#15026) ;
#4541 = VERTEX_POINT('',#15084) ;
#4542 = VERTEX_POINT('',#15086) ;
#4543 = VERTEX_POINT('',#15090) ;
#4544 = VERTEX_POINT('',#15091) ;
#4545 = VERTEX_POINT('',#15093) ;
#4546 = VERTEX_POINT('',#15095) ;
#4547 = VERTEX_POINT('',#15097) ;
#4548 = VERTEX_POINT('',#15099) ;
#4549 = VERTEX_POINT('',#15103) ;
#4550 = VERTEX_POINT('',#15105) ;
#4551 = VERTEX_POINT('',#15109) ;
#4552 = VERTEX_POINT('',#15110) ;
#4553 = VERTEX_POINT('',#15115) ;
#4554 = VERTEX_POINT('',#15121) ;
#4555 = VERTEX_POINT('',#15127) ;
#4556 = VERTEX_POINT('',#15130) ;
#4557 = VERTEX_POINT('',#15132) ;
#4558 = VERTEX_POINT('',#15136) ;
#4559 = VERTEX_POINT('',#15138) ;
#4560 = VERTEX_POINT('',#15142) ;
#4561 = VERTEX_POINT('',#15144) ;
#4562 = VERTEX_POINT('',#15148) ;
#4563 = VERTEX_POINT('',#15150) ;
#4564 = VERTEX_POINT('',#15155) ;
#4565 = VERTEX_POINT('',#15162) ;
#4566 = VERTEX_POINT('',#15164) ;
#4567 = VERTEX_POINT('',#15168) ;
#4568 = VERTEX_POINT('',#15169) ;
#4569 = VERTEX_POINT('',#15171) ;
#4570 = VERTEX_POINT('',#15173) ;
#4571 = VERTEX_POINT('',#15177) ;
#4572 = VERTEX_POINT('',#15179) ;
#4573 = VERTEX_POINT('',#15183) ;
#4574 = VERTEX_POINT('',#15185) ;
#4575 = VERTEX_POINT('',#15195) ;
#4576 = VERTEX_POINT('',#15198) ;
#4577 = VERTEX_POINT('',#15202) ;
#4578 = VERTEX_POINT('',#15206) ;
#4579 = VERTEX_POINT('',#15209) ;
#4580 = VERTEX_POINT('',#15213) ;
#4581 = VERTEX_POINT('',#15216) ;
#4582 = VERTEX_POINT('',#15220) ;
#4583 = VERTEX_POINT('',#15223) ;
#4584 = VERTEX_POINT('',#15227) ;
#4585 = VERTEX_POINT('',#15233) ;
#4586 = VERTEX_POINT('',#15234) ;
#4587 = VERTEX_POINT('',#15236) ;
#4588 = VERTEX_POINT('',#15238) ;
#4589 = VERTEX_POINT('',#15242) ;
#4590 = VERTEX_POINT('',#15243) ;
#4591 = VERTEX_POINT('',#15245) ;
#4592 = VERTEX_POINT('',#15247) ;
#4593 = VERTEX_POINT('',#15251) ;
#4594 = VERTEX_POINT('',#15253) ;
#4595 = VERTEX_POINT('',#15257) ;
#4596 = VERTEX_POINT('',#15259) ;
#4597 = VERTEX_POINT('',#15272) ;
#4598 = VERTEX_POINT('',#15275) ;
#4599 = VERTEX_POINT('',#15279) ;
#4600 = VERTEX_POINT('',#15283) ;
#4601 = VERTEX_POINT('',#15287) ;
#4602 = VERTEX_POINT('',#15290) ;
#4603 = VERTEX_POINT('',#15294) ;
#4604 = VERTEX_POINT('',#15300) ;
#4605 = VERTEX_POINT('',#15301) ;
#4606 = VERTEX_POINT('',#15303) ;
#4607 = VERTEX_POINT('',#15314) ;
#4608 = VERTEX_POINT('',#15324) ;
#4609 = VERTEX_POINT('',#15325) ;
#4610 = VERTEX_POINT('',#15372) ;
#4611 = VERTEX_POINT('',#15373) ;
#4612 = VERTEX_POINT('',#15420) ;
#4613 = VERTEX_POINT('',#15421) ;
#4614 = VERTEX_POINT('',#15474) ;
#4615 = VERTEX_POINT('',#15475) ;
#4616 = VERTEX_POINT('',#15522) ;
#4617 = VERTEX_POINT('',#15523) ;
#4618 = VERTEX_POINT('',#15570) ;
#4619 = VERTEX_POINT('',#15571) ;
#4620 = VERTEX_POINT('',#15624) ;
#4621 = VERTEX_POINT('',#15625) ;
#4622 = VERTEX_POINT('',#15672) ;
#4623 = VERTEX_POINT('',#15673) ;
#4624 = VERTEX_POINT('',#15720) ;
#4625 = VERTEX_POINT('',#15721) ;
#4626 = VERTEX_POINT('',#15774) ;
#4627 = VERTEX_POINT('',#15775) ;
#4628 = VERTEX_POINT('',#15822) ;
#4629 = VERTEX_POINT('',#15823) ;
#4630 = VERTEX_POINT('',#15870) ;
#4631 = VERTEX_POINT('',#15871) ;
#4632 = VERTEX_POINT('',#15924) ;
#4633 = VERTEX_POINT('',#15925) ;
#4634 = VERTEX_POINT('',#15972) ;
#4635 = VERTEX_POINT('',#15973) ;
#4636 = VERTEX_POINT('',#15975) ;
#4637 = VERTEX_POINT('',#15981) ;
#4638 = VERTEX_POINT('',#15988) ;
#4639 = VERTEX_POINT('',#15989) ;
#4640 = VERTEX_POINT('',#16012) ;
#4641 = VERTEX_POINT('',#16013) ;
#4642 = VERTEX_POINT('',#16037) ;
#4643 = VERTEX_POINT('',#16038) ;
#4644 = VERTEX_POINT('',#16062) ;
#4645 = VERTEX_POINT('',#16063) ;
#4646 = VERTEX_POINT('',#16086) ;
#4647 = VERTEX_POINT('',#16087) ;
#4648 = VERTEX_POINT('',#16111) ;
#4649 = VERTEX_POINT('',#16112) ;
#4650 = VERTEX_POINT('',#16136) ;
#4651 = VERTEX_POINT('',#16137) ;
#4652 = VERTEX_POINT('',#16160) ;
#4653 = VERTEX_POINT('',#16161) ;
#4654 = VERTEX_POINT('',#16185) ;
#4655 = VERTEX_POINT('',#16186) ;
#4656 = VERTEX_POINT('',#16210) ;
#4657 = VERTEX_POINT('',#16211) ;
#4658 = VERTEX_POINT('',#16234) ;
#4659 = VERTEX_POINT('',#16235) ;
#4660 = VERTEX_POINT('',#16259) ;
#4661 = VERTEX_POINT('',#16260) ;
#4662 = VERTEX_POINT('',#16284) ;
#4663 = VERTEX_POINT('',#16285) ;
#4664 = VERTEX_POINT('',#16308) ;
#4665 = VERTEX_POINT('',#16382) ;
#4666 = VERTEX_POINT('',#16384) ;
#4667 = VERTEX_POINT('',#16850) ;
#4668 = VERTEX_POINT('',#16934) ;
#4669 = VERTEX_POINT('',#16936) ;
#4670 = VERTEX_POINT('',#17410) ;
#4671 = VERTEX_POINT('',#17416) ;
#4672 = VERTEX_POINT('',#17419) ;
#4673 = VERTEX_POINT('',#17424) ;
#4674 = VERTEX_POINT('',#17425) ;
#4675 = VERTEX_POINT('',#17427) ;
#4676 = VERTEX_POINT('',#17431) ;
#4677 = VERTEX_POINT('',#17433) ;
#4678 = VERTEX_POINT('',#17439) ;
#4679 = VERTEX_POINT('',#17445) ;
#4680 = VERTEX_POINT('',#17447) ;
#4681 = VERTEX_POINT('',#17449) ;
#4682 = VERTEX_POINT('',#17451) ;
#4683 = VERTEX_POINT('',#17453) ;
#4684 = VERTEX_POINT('',#17455) ;
#4685 = VERTEX_POINT('',#17457) ;
#4686 = VERTEX_POINT('',#17459) ;
#4687 = VERTEX_POINT('',#17461) ;
#4688 = VERTEX_POINT('',#17463) ;
#4689 = VERTEX_POINT('',#17465) ;
#4690 = VERTEX_POINT('',#17467) ;
#4691 = VERTEX_POINT('',#17469) ;
#4692 = VERTEX_POINT('',#17471) ;
#4693 = VERTEX_POINT('',#17473) ;
#4694 = VERTEX_POINT('',#17475) ;
#4695 = VERTEX_POINT('',#17477) ;
#4696 = VERTEX_POINT('',#17479) ;
#4697 = VERTEX_POINT('',#17481) ;
#4698 = VERTEX_POINT('',#17483) ;
#4699 = VERTEX_POINT('',#17485) ;
#4700 = VERTEX_POINT('',#17487) ;
#4701 = VERTEX_POINT('',#17489) ;
#4702 = VERTEX_POINT('',#17491) ;
#4703 = VERTEX_POINT('',#17493) ;
#4704 = VERTEX_POINT('',#17495) ;
#4705 = VERTEX_POINT('',#17497) ;
#4706 = VERTEX_POINT('',#17499) ;
#4707 = VERTEX_POINT('',#17501) ;
#4708 = VERTEX_POINT('',#17503) ;
#4709 = VERTEX_POINT('',#17505) ;
#4710 = VERTEX_POINT('',#17507) ;
#4711 = VERTEX_POINT('',#17509) ;
#4712 = VERTEX_POINT('',#17511) ;
#4713 = VERTEX_POINT('',#17513) ;
#4714 = VERTEX_POINT('',#17515) ;
#4715 = VERTEX_POINT('',#17517) ;
#4716 = VERTEX_POINT('',#17519) ;
#4717 = VERTEX_POINT('',#17521) ;
#4718 = VERTEX_POINT('',#17523) ;
#4719 = VERTEX_POINT('',#17525) ;
#4720 = VERTEX_POINT('',#17527) ;
#4721 = VERTEX_POINT('',#17529) ;
#4722 = VERTEX_POINT('',#17531) ;
#4723 = VERTEX_POINT('',#17533) ;
#4724 = VERTEX_POINT('',#17535) ;
#4725 = VERTEX_POINT('',#17537) ;
#4726 = VERTEX_POINT('',#17539) ;
#4727 = VERTEX_POINT('',#17541) ;
#4728 = VERTEX_POINT('',#17543) ;
#4729 = VERTEX_POINT('',#17545) ;
#4730 = VERTEX_POINT('',#17547) ;
#4731 = VERTEX_POINT('',#17549) ;
#4732 = VERTEX_POINT('',#17551) ;
#4733 = VERTEX_POINT('',#17553) ;
#4734 = VERTEX_POINT('',#17555) ;
#4735 = VERTEX_POINT('',#17557) ;
#4736 = VERTEX_POINT('',#17559) ;
#4737 = VERTEX_POINT('',#17561) ;
#4738 = VERTEX_POINT('',#17563) ;
#4739 = VERTEX_POINT('',#17565) ;
#4740 = VERTEX_POINT('',#17567) ;
#4741 = VERTEX_POINT('',#17569) ;
#4742 = VERTEX_POINT('',#17571) ;
#4743 = VERTEX_POINT('',#17573) ;
#4744 = VERTEX_POINT('',#17575) ;
#4745 = VERTEX_POINT('',#17577) ;
#4746 = VERTEX_POINT('',#17579) ;
#4747 = VERTEX_POINT('',#17581) ;
#4748 = VERTEX_POINT('',#17583) ;
#4749 = VERTEX_POINT('',#17585) ;
#4750 = VERTEX_POINT('',#17587) ;
#4751 = VERTEX_POINT('',#17589) ;
#4752 = VERTEX_POINT('',#17591) ;
#4753 = VERTEX_POINT('',#17593) ;
#4754 = VERTEX_POINT('',#17595) ;
#4755 = VERTEX_POINT('',#17598) ;
#4756 = VERTEX_POINT('',#17600) ;
#4757 = VERTEX_POINT('',#17602) ;
#4758 = VERTEX_POINT('',#17604) ;
#4759 = VERTEX_POINT('',#17606) ;
#4760 = VERTEX_POINT('',#17608) ;
#4761 = VERTEX_POINT('',#17610) ;
#4762 = VERTEX_POINT('',#17612) ;
#4763 = VERTEX_POINT('',#17614) ;
#4764 = VERTEX_POINT('',#17616) ;
#4765 = VERTEX_POINT('',#17618) ;
#4766 = VERTEX_POINT('',#17620) ;
#4767 = VERTEX_POINT('',#17622) ;
#4768 = VERTEX_POINT('',#17624) ;
#4769 = VERTEX_POINT('',#17626) ;
#4770 = VERTEX_POINT('',#17628) ;
#4771 = VERTEX_POINT('',#17630) ;
#4772 = VERTEX_POINT('',#17632) ;
#4773 = VERTEX_POINT('',#17634) ;
#4774 = VERTEX_POINT('',#17636) ;
#4775 = VERTEX_POINT('',#17638) ;
#4776 = VERTEX_POINT('',#17640) ;
#4777 = VERTEX_POINT('',#17642) ;
#4778 = VERTEX_POINT('',#17644) ;
#4779 = VERTEX_POINT('',#17646) ;
#4780 = VERTEX_POINT('',#17648) ;
#4781 = VERTEX_POINT('',#17650) ;
#4782 = VERTEX_POINT('',#17652) ;
#4783 = VERTEX_POINT('',#17654) ;
#4784 = VERTEX_POINT('',#17656) ;
#4785 = VERTEX_POINT('',#17658) ;
#4786 = VERTEX_POINT('',#17660) ;
#4787 = VERTEX_POINT('',#17662) ;
#4788 = VERTEX_POINT('',#17664) ;
#4789 = VERTEX_POINT('',#17666) ;
#4790 = VERTEX_POINT('',#17668) ;
#4791 = VERTEX_POINT('',#17670) ;
#4792 = VERTEX_POINT('',#17672) ;
#4793 = VERTEX_POINT('',#17674) ;
#4794 = VERTEX_POINT('',#17676) ;
#4795 = VERTEX_POINT('',#17678) ;
#4796 = VERTEX_POINT('',#17680) ;
#4797 = VERTEX_POINT('',#17682) ;
#4798 = VERTEX_POINT('',#17684) ;
#4799 = VERTEX_POINT('',#17686) ;
#4800 = VERTEX_POINT('',#17688) ;
#4801 = VERTEX_POINT('',#17690) ;
#4802 = VERTEX_POINT('',#17692) ;
#4803 = VERTEX_POINT('',#17694) ;
#4804 = VERTEX_POINT('',#17696) ;
#4805 = VERTEX_POINT('',#17698) ;
#4806 = VERTEX_POINT('',#17700) ;
#4807 = VERTEX_POINT('',#17702) ;
#4808 = VERTEX_POINT('',#17704) ;
#4809 = VERTEX_POINT('',#17706) ;
#4810 = VERTEX_POINT('',#17708) ;
#4811 = VERTEX_POINT('',#17710) ;
#4812 = VERTEX_POINT('',#17712) ;
#4813 = VERTEX_POINT('',#17714) ;
#4814 = VERTEX_POINT('',#17716) ;
#4815 = VERTEX_POINT('',#17718) ;
#4816 = VERTEX_POINT('',#17720) ;
#4817 = VERTEX_POINT('',#17722) ;
#4818 = VERTEX_POINT('',#17724) ;
#4819 = VERTEX_POINT('',#17726) ;
#4820 = VERTEX_POINT('',#17728) ;
#4821 = VERTEX_POINT('',#17732) ;
#4822 = VERTEX_POINT('',#17734) ;
#4823 = VERTEX_POINT('',#17746) ;
#4824 = VERTEX_POINT('',#17748) ;
#4825 = VERTEX_POINT('',#17753) ;
#4826 = VERTEX_POINT('',#17760) ;
#4827 = VERTEX_POINT('',#17767) ;
#4828 = VERTEX_POINT('',#17774) ;
#4829 = VERTEX_POINT('',#17781) ;
#4830 = VERTEX_POINT('',#17788) ;
#4831 = VERTEX_POINT('',#17795) ;
#4832 = VERTEX_POINT('',#17802) ;
#4833 = VERTEX_POINT('',#17809) ;
#4834 = VERTEX_POINT('',#17816) ;
#4835 = VERTEX_POINT('',#17823) ;
#4836 = VERTEX_POINT('',#17830) ;
#4837 = VERTEX_POINT('',#17837) ;
#4838 = VERTEX_POINT('',#17844) ;
#4839 = VERTEX_POINT('',#17851) ;
#4840 = VERTEX_POINT('',#17858) ;
#4841 = VERTEX_POINT('',#17865) ;
#4842 = VERTEX_POINT('',#17872) ;
#4843 = VERTEX_POINT('',#17879) ;
#4844 = VERTEX_POINT('',#17886) ;
#4845 = VERTEX_POINT('',#17893) ;
#4846 = VERTEX_POINT('',#17900) ;
#4847 = VERTEX_POINT('',#17907) ;
#4848 = VERTEX_POINT('',#17914) ;
#4849 = VERTEX_POINT('',#17921) ;
#4850 = VERTEX_POINT('',#17928) ;
#4851 = VERTEX_POINT('',#17935) ;
#4852 = VERTEX_POINT('',#17942) ;
#4853 = VERTEX_POINT('',#17949) ;
#4854 = VERTEX_POINT('',#17956) ;
#4855 = VERTEX_POINT('',#17963) ;
#4856 = VERTEX_POINT('',#17970) ;
#4857 = VERTEX_POINT('',#17977) ;
#4858 = VERTEX_POINT('',#17988) ;
#4859 = VERTEX_POINT('',#17995) ;
#4860 = VERTEX_POINT('',#18002) ;
#4861 = VERTEX_POINT('',#18009) ;
#4862 = VERTEX_POINT('',#18016) ;
#4863 = VERTEX_POINT('',#18023) ;
#4864 = VERTEX_POINT('',#18030) ;
#4865 = VERTEX_POINT('',#18037) ;
#4866 = VERTEX_POINT('',#18044) ;
#4867 = VERTEX_POINT('',#18051) ;
#4868 = VERTEX_POINT('',#18058) ;
#4869 = VERTEX_POINT('',#18065) ;
#4870 = VERTEX_POINT('',#18072) ;
#4871 = VERTEX_POINT('',#18079) ;
#4872 = VERTEX_POINT('',#18086) ;
#4873 = VERTEX_POINT('',#18093) ;
#4874 = VERTEX_POINT('',#18100) ;
#4875 = VERTEX_POINT('',#18107) ;
#4876 = VERTEX_POINT('',#18114) ;
#4877 = VERTEX_POINT('',#18121) ;
#4878 = VERTEX_POINT('',#18128) ;
#4879 = VERTEX_POINT('',#18135) ;
#4880 = VERTEX_POINT('',#18142) ;
#4881 = VERTEX_POINT('',#18149) ;
#4882 = VERTEX_POINT('',#18156) ;
#4883 = VERTEX_POINT('',#18163) ;
#4884 = VERTEX_POINT('',#18170) ;
#4885 = VERTEX_POINT('',#18177) ;
#4886 = VERTEX_POINT('',#18184) ;
#4887 = VERTEX_POINT('',#18191) ;
#4888 = VERTEX_POINT('',#18198) ;
#4889 = VERTEX_POINT('',#18205) ;
#4890 = VERTEX_POINT('',#18212) ;
#4891 = VERTEX_POINT('',#18219) ;
#4892 = VERTEX_POINT('',#18228) ;
#4893 = VERTEX_POINT('',#18231) ;
#4894 = VERTEX_POINT('',#18233) ;
#4895 = VERTEX_POINT('',#18237) ;
#4896 = VERTEX_POINT('',#18239) ;
#4897 = VERTEX_POINT('',#18243) ;
#4898 = VERTEX_POINT('',#18247) ;
#4899 = VERTEX_POINT('',#18249) ;
#4900 = VERTEX_POINT('',#18253) ;
#4901 = VERTEX_POINT('',#18257) ;
#4902 = VERTEX_POINT('',#18259) ;
#4903 = VERTEX_POINT('',#18263) ;
#4904 = VERTEX_POINT('',#18267) ;
#4905 = VERTEX_POINT('',#18269) ;
#4906 = VERTEX_POINT('',#18273) ;
#4907 = VERTEX_POINT('',#18277) ;
#4908 = VERTEX_POINT('',#18279) ;
#4909 = VERTEX_POINT('',#18283) ;
#4910 = VERTEX_POINT('',#18287) ;
#4911 = VERTEX_POINT('',#18293) ;
#4912 = VERTEX_POINT('',#18295) ;
#4913 = VERTEX_POINT('',#18299) ;
#4914 = VERTEX_POINT('',#18301) ;
#4915 = VERTEX_POINT('',#18305) ;
#4916 = VERTEX_POINT('',#18307) ;
#4917 = VERTEX_POINT('',#18311) ;
#4918 = VERTEX_POINT('',#18313) ;
#4919 = VERTEX_POINT('',#18317) ;
#4920 = VERTEX_POINT('',#18319) ;
#4921 = VERTEX_POINT('',#18323) ;
#4922 = VERTEX_POINT('',#18325) ;
#4923 = VERTEX_POINT('',#18330) ;
#4924 = VERTEX_POINT('',#18332) ;
#4925 = VERTEX_POINT('',#18337) ;
#4926 = VERTEX_POINT('',#18342) ;
#4927 = VERTEX_POINT('',#18355) ;
#4928 = VERTEX_POINT('',#18365) ;
#4929 = VERTEX_POINT('',#18372) ;
#4930 = VERTEX_POINT('',#18381) ;
#4931 = VERTEX_POINT('',#18383) ;
#4932 = VERTEX_POINT('',#18387) ;
#4933 = VERTEX_POINT('',#18389) ;
#4934 = VERTEX_POINT('',#18393) ;
#4935 = VERTEX_POINT('',#18394) ;
#4936 = VERTEX_POINT('',#18396) ;
#4937 = VERTEX_POINT('',#18398) ;
#4938 = VERTEX_POINT('',#18400) ;
#4939 = VERTEX_POINT('',#18402) ;
#4940 = VERTEX_POINT('',#18406) ;
#4941 = VERTEX_POINT('',#18408) ;
#4942 = VERTEX_POINT('',#18412) ;
#4943 = VERTEX_POINT('',#18414) ;
#4944 = VERTEX_POINT('',#18418) ;
#4945 = VERTEX_POINT('',#18420) ;
#4946 = VERTEX_POINT('',#18427) ;
#4947 = VERTEX_POINT('',#18429) ;
#4948 = VERTEX_POINT('',#18434) ;
#4949 = VERTEX_POINT('',#18436) ;
#4950 = VERTEX_POINT('',#18438) ;
#4951 = VERTEX_POINT('',#18442) ;
#4952 = VERTEX_POINT('',#18444) ;
#4953 = VERTEX_POINT('',#18446) ;
#4954 = VERTEX_POINT('',#18448) ;
#4955 = VERTEX_POINT('',#18450) ;
#4956 = VERTEX_POINT('',#18452) ;
#4957 = VERTEX_POINT('',#18455) ;
#4958 = VERTEX_POINT('',#18458) ;
#4959 = VERTEX_POINT('',#18462) ;
#4960 = VERTEX_POINT('',#18464) ;
#4961 = VERTEX_POINT('',#18468) ;
#4962 = VERTEX_POINT('',#18472) ;
#4963 = VERTEX_POINT('',#18480) ;
#4964 = VERTEX_POINT('',#18484) ;
#4965 = VERTEX_POINT('',#18487) ;
#4966 = VERTEX_POINT('',#18491) ;
#4967 = VERTEX_POINT('',#18492) ;
#4968 = VERTEX_POINT('',#18494) ;
#4969 = VERTEX_POINT('',#18496) ;
#4970 = VERTEX_POINT('',#18500) ;
#4971 = VERTEX_POINT('',#18502) ;
#4972 = VERTEX_POINT('',#18506) ;
#4973 = VERTEX_POINT('',#18508) ;
#4974 = VERTEX_POINT('',#18518) ;
#4975 = VERTEX_POINT('',#18520) ;
#4976 = VERTEX_POINT('',#18524) ;
#4977 = VERTEX_POINT('',#18526) ;
#4978 = VERTEX_POINT('',#18530) ;
#4979 = VERTEX_POINT('',#18531) ;
#4980 = VERTEX_POINT('',#18533) ;
#4981 = VERTEX_POINT('',#18535) ;
#4982 = VERTEX_POINT('',#18538) ;
#4983 = VERTEX_POINT('',#18541) ;
#4984 = VERTEX_POINT('',#18543) ;
#4985 = VERTEX_POINT('',#18547) ;
#4986 = VERTEX_POINT('',#18551) ;
#4987 = VERTEX_POINT('',#18553) ;
#4988 = VERTEX_POINT('',#18561) ;
#4989 = VERTEX_POINT('',#18562) ;
#4990 = VERTEX_POINT('',#18564) ;
#4991 = VERTEX_POINT('',#18566) ;
#4992 = VERTEX_POINT('',#18569) ;
#4993 = VERTEX_POINT('',#18572) ;
#4994 = VERTEX_POINT('',#18574) ;
#4995 = VERTEX_POINT('',#18578) ;
#4996 = VERTEX_POINT('',#18582) ;
#4997 = VERTEX_POINT('',#18584) ;
#4998 = VERTEX_POINT('',#18592) ;
#4999 = VERTEX_POINT('',#18593) ;
#5000 = VERTEX_POINT('',#18595) ;
#5001 = VERTEX_POINT('',#18597) ;
#5002 = VERTEX_POINT('',#18601) ;
#5003 = VERTEX_POINT('',#18603) ;
#5004 = VERTEX_POINT('',#18607) ;
#5005 = VERTEX_POINT('',#18609) ;
#5006 = VERTEX_POINT('',#18619) ;
#5007 = VERTEX_POINT('',#18621) ;
#5008 = VERTEX_POINT('',#18624) ;
#5009 = VERTEX_POINT('',#18628) ;
#5010 = VERTEX_POINT('',#18631) ;
#5011 = VERTEX_POINT('',#18635) ;
#5012 = VERTEX_POINT('',#18639) ;
#5013 = VERTEX_POINT('',#18643) ;
#5014 = VERTEX_POINT('',#18647) ;
#5015 = VERTEX_POINT('',#18651) ;
#5016 = VERTEX_POINT('',#18654) ;
#5017 = VERTEX_POINT('',#18658) ;
#5018 = EDGE_CURVE('',#4150,#4150,#3775,.T.) ;
#5019 = EDGE_CURVE('',#4150,#4151,#2233,.T.) ;
#5020 = EDGE_CURVE('',#4151,#4151,#3776,.T.) ;
#5021 = EDGE_CURVE('',#4152,#4153,#2234,.T.) ;
#5022 = EDGE_CURVE('',#4154,#4152,#2235,.T.) ;
#5023 = EDGE_CURVE('',#4155,#4154,#2236,.T.) ;
#5024 = EDGE_CURVE('',#4153,#4155,#2237,.T.) ;
#5025 = EDGE_CURVE('',#4156,#4156,#3777,.T.) ;
#5026 = EDGE_CURVE('',#4151,#4157,#2238,.T.) ;
#5027 = EDGE_CURVE('',#4157,#4157,#3778,.T.) ;
#5028 = EDGE_CURVE('',#4158,#4158,#3779,.T.) ;
#5029 = EDGE_CURVE('',#4158,#4159,#2239,.T.) ;
#5030 = EDGE_CURVE('',#4159,#4159,#3780,.T.) ;
#5031 = EDGE_CURVE('',#4160,#4161,#2240,.T.) ;
#5032 = EDGE_CURVE('',#4162,#4160,#2241,.T.) ;
#5033 = EDGE_CURVE('',#4163,#4162,#2242,.T.) ;
#5034 = EDGE_CURVE('',#4161,#4163,#2243,.T.) ;
#5035 = EDGE_CURVE('',#4164,#4164,#3781,.T.) ;
#5036 = EDGE_CURVE('',#4159,#4165,#2244,.T.) ;
#5037 = EDGE_CURVE('',#4165,#4165,#3782,.T.) ;
#5038 = EDGE_CURVE('',#4166,#4166,#3783,.T.) ;
#5039 = EDGE_CURVE('',#4166,#4167,#2245,.T.) ;
#5040 = EDGE_CURVE('',#4167,#4167,#3784,.T.) ;
#5041 = EDGE_CURVE('',#4168,#4169,#2246,.T.) ;
#5042 = EDGE_CURVE('',#4170,#4168,#2247,.T.) ;
#5043 = EDGE_CURVE('',#4171,#4170,#2248,.T.) ;
#5044 = EDGE_CURVE('',#4169,#4171,#2249,.T.) ;
#5045 = EDGE_CURVE('',#4172,#4172,#3785,.T.) ;
#5046 = EDGE_CURVE('',#4167,#4173,#2250,.T.) ;
#5047 = EDGE_CURVE('',#4173,#4173,#3786,.T.) ;
#5048 = EDGE_CURVE('',#4174,#4174,#3787,.T.) ;
#5049 = EDGE_CURVE('',#4174,#4175,#2251,.T.) ;
#5050 = EDGE_CURVE('',#4175,#4175,#3788,.T.) ;
#5051 = EDGE_CURVE('',#4176,#4177,#2252,.T.) ;
#5052 = EDGE_CURVE('',#4178,#4176,#2253,.T.) ;
#5053 = EDGE_CURVE('',#4179,#4178,#2254,.T.) ;
#5054 = EDGE_CURVE('',#4177,#4179,#2255,.T.) ;
#5055 = EDGE_CURVE('',#4180,#4180,#3789,.T.) ;
#5056 = EDGE_CURVE('',#4175,#4181,#2256,.T.) ;
#5057 = EDGE_CURVE('',#4181,#4181,#3790,.T.) ;
#5058 = EDGE_CURVE('',#4172,#4182,#2257,.T.) ;
#5059 = EDGE_CURVE('',#4182,#4182,#3791,.T.) ;
#5060 = EDGE_CURVE('',#4182,#4183,#2258,.T.) ;
#5061 = EDGE_CURVE('',#4183,#4184,#3792,.T.) ;
#5062 = EDGE_CURVE('',#4185,#4184,#407,.T.) ;
#5063 = EDGE_CURVE('',#4185,#4183,#3793,.T.) ;
#5064 = EDGE_CURVE('',#4180,#4186,#2259,.T.) ;
#5065 = EDGE_CURVE('',#4186,#4186,#3794,.T.) ;
#5066 = EDGE_CURVE('',#4186,#4187,#2260,.T.) ;
#5067 = EDGE_CURVE('',#4187,#4188,#3795,.T.) ;
#5068 = EDGE_CURVE('',#4189,#4188,#408,.T.) ;
#5069 = EDGE_CURVE('',#4189,#4187,#3796,.T.) ;
#5070 = EDGE_CURVE('',#4164,#4190,#2261,.T.) ;
#5071 = EDGE_CURVE('',#4190,#4190,#3797,.T.) ;
#5072 = EDGE_CURVE('',#4190,#4191,#2262,.T.) ;
#5073 = EDGE_CURVE('',#4191,#4191,#3798,.T.) ;
#5074 = EDGE_CURVE('',#4156,#4192,#2263,.T.) ;
#5075 = EDGE_CURVE('',#4192,#4192,#3799,.T.) ;
#5076 = EDGE_CURVE('',#4192,#4193,#2264,.T.) ;
#5077 = EDGE_CURVE('',#4193,#4193,#3800,.T.) ;
#5078 = EDGE_CURVE('',#4157,#4194,#2265,.T.) ;
#5079 = EDGE_CURVE('',#4193,#4195,#2266,.T.) ;
#5080 = EDGE_CURVE('',#4165,#4196,#2267,.T.) ;
#5081 = EDGE_CURVE('',#4191,#4197,#2268,.T.) ;
#5082 = EDGE_CURVE('',#4188,#4189,#409,.T.) ;
#5083 = EDGE_CURVE('',#4198,#4198,#3801,.T.) ;
#5084 = EDGE_CURVE('',#4198,#4199,#2269,.T.) ;
#5085 = EDGE_CURVE('',#4199,#4199,#3802,.T.) ;
#5086 = EDGE_CURVE('',#4181,#4200,#2270,.T.) ;
#5087 = EDGE_CURVE('',#4184,#4185,#410,.T.) ;
#5088 = EDGE_CURVE('',#4201,#4201,#3803,.T.) ;
#5089 = EDGE_CURVE('',#4201,#4202,#2271,.T.) ;
#5090 = EDGE_CURVE('',#4202,#4202,#3804,.T.) ;
#5091 = EDGE_CURVE('',#4173,#4203,#2272,.T.) ;
#5092 = EDGE_CURVE('',#4204,#4205,#411,.T.) ;
#5093 = EDGE_CURVE('',#4205,#4204,#412,.T.) ;
#5094 = EDGE_CURVE('',#4205,#4206,#2273,.T.) ;
#5095 = EDGE_CURVE('',#4207,#4206,#413,.T.) ;
#5096 = EDGE_CURVE('',#4206,#4207,#414,.T.) ;
#5097 = EDGE_CURVE('',#4208,#4208,#3805,.T.) ;
#5098 = EDGE_CURVE('',#4208,#4209,#2274,.T.) ;
#5099 = EDGE_CURVE('',#4209,#4209,#3806,.T.) ;
#5100 = EDGE_CURVE('',#4210,#4211,#415,.T.) ;
#5101 = EDGE_CURVE('',#4211,#4210,#416,.T.) ;
#5102 = EDGE_CURVE('',#4211,#4212,#2275,.T.) ;
#5103 = EDGE_CURVE('',#4213,#4212,#417,.T.) ;
#5104 = EDGE_CURVE('',#4212,#4213,#418,.T.) ;
#5105 = EDGE_CURVE('',#4214,#4214,#3807,.T.) ;
#5106 = EDGE_CURVE('',#4214,#4215,#2276,.T.) ;
#5107 = EDGE_CURVE('',#4215,#4215,#3808,.T.) ;
#5108 = EDGE_CURVE('',#4216,#4216,#3809,.T.) ;
#5109 = EDGE_CURVE('',#4216,#4217,#2277,.T.) ;
#5110 = EDGE_CURVE('',#4217,#4217,#3810,.T.) ;
#5111 = EDGE_CURVE('',#4218,#4218,#3811,.T.) ;
#5112 = EDGE_CURVE('',#4218,#4219,#2278,.T.) ;
#5113 = EDGE_CURVE('',#4219,#4219,#3812,.T.) ;
#5114 = EDGE_CURVE('',#4220,#4221,#2279,.T.) ;
#5115 = EDGE_CURVE('',#4222,#4220,#3813,.T.) ;
#5116 = EDGE_CURVE('',#4223,#4222,#2280,.T.) ;
#5117 = EDGE_CURVE('',#4221,#4223,#3814,.T.) ;
#5118 = EDGE_CURVE('',#4224,#4225,#2281,.T.) ;
#5119 = EDGE_CURVE('',#4226,#4224,#3815,.T.) ;
#5120 = EDGE_CURVE('',#4227,#4226,#2282,.T.) ;
#5121 = EDGE_CURVE('',#4225,#4227,#3816,.T.) ;
#5122 = EDGE_CURVE('',#4228,#4226,#2283,.T.) ;
#5123 = EDGE_CURVE('',#4229,#4228,#2284,.T.) ;
#5124 = EDGE_CURVE('',#4229,#4227,#2285,.T.) ;
#5125 = EDGE_CURVE('',#4224,#4230,#3817,.T.) ;
#5126 = EDGE_CURVE('',#4230,#4231,#2286,.T.) ;
#5127 = EDGE_CURVE('',#4232,#4231,#2287,.T.) ;
#5128 = EDGE_CURVE('',#4232,#4228,#2288,.T.) ;
#5129 = EDGE_CURVE('',#4233,#4222,#2289,.T.) ;
#5130 = EDGE_CURVE('',#4234,#4233,#2290,.T.) ;
#5131 = EDGE_CURVE('',#4234,#4223,#2291,.T.) ;
#5132 = EDGE_CURVE('',#4220,#4235,#3818,.T.) ;
#5133 = EDGE_CURVE('',#4235,#4236,#2292,.T.) ;
#5134 = EDGE_CURVE('',#4237,#4236,#2293,.T.) ;
#5135 = EDGE_CURVE('',#4237,#4233,#2294,.T.) ;
#5136 = EDGE_CURVE('',#4238,#4239,#2295,.T.) ;
#5137 = EDGE_CURVE('',#4239,#4240,#2296,.T.) ;
#5138 = EDGE_CURVE('',#4240,#4241,#2297,.T.) ;
#5139 = EDGE_CURVE('',#4241,#4238,#2298,.T.) ;
#5140 = EDGE_CURVE('',#4242,#4241,#2299,.T.) ;
#5141 = EDGE_CURVE('',#4242,#4243,#2300,.T.) ;
#5142 = EDGE_CURVE('',#4243,#4244,#2301,.T.) ;
#5143 = EDGE_CURVE('',#4244,#4245,#2302,.T.) ;
#5144 = EDGE_CURVE('',#4245,#4238,#2303,.T.) ;
#5145 = EDGE_CURVE('',#4246,#4240,#2304,.T.) ;
#5146 = EDGE_CURVE('',#4246,#4247,#2305,.T.) ;
#5147 = EDGE_CURVE('',#4247,#4248,#2306,.T.) ;
#5148 = EDGE_CURVE('',#4248,#4249,#2307,.T.) ;
#5149 = EDGE_CURVE('',#4250,#4249,#2308,.T.) ;
#5150 = EDGE_CURVE('',#4250,#4251,#2309,.T.) ;
#5151 = EDGE_CURVE('',#4251,#4252,#2310,.T.) ;
#5152 = EDGE_CURVE('',#4252,#4253,#2311,.T.) ;
#5153 = EDGE_CURVE('',#4254,#4253,#2312,.T.) ;
#5154 = EDGE_CURVE('',#4255,#4254,#2313,.T.) ;
#5155 = EDGE_CURVE('',#4256,#4255,#2314,.T.) ;
#5156 = EDGE_CURVE('',#4257,#4256,#2315,.T.) ;
#5157 = EDGE_CURVE('',#4179,#4257,#2316,.T.) ;
#5158 = EDGE_CURVE('',#4178,#4258,#2317,.T.) ;
#5159 = EDGE_CURVE('',#4258,#4259,#2318,.T.) ;
#5160 = EDGE_CURVE('',#4171,#4259,#2319,.T.) ;
#5161 = EDGE_CURVE('',#4170,#4260,#2320,.T.) ;
#5162 = EDGE_CURVE('',#4242,#4260,#2321,.T.) ;
#5163 = EDGE_CURVE('',#4254,#4261,#2322,.T.) ;
#5164 = EDGE_CURVE('',#4261,#4262,#2323,.T.) ;
#5165 = EDGE_CURVE('',#4262,#4255,#2324,.T.) ;
#5166 = EDGE_CURVE('',#4263,#4262,#2325,.T.) ;
#5167 = EDGE_CURVE('',#4263,#4264,#2326,.T.) ;
#5168 = EDGE_CURVE('',#4264,#4265,#2327,.T.) ;
#5169 = EDGE_CURVE('',#4265,#4256,#2328,.T.) ;
#5170 = EDGE_CURVE('',#4266,#4266,#3819,.T.) ;
#5171 = EDGE_CURVE('',#4266,#4267,#2329,.T.) ;
#5172 = EDGE_CURVE('',#4267,#4268,#3820,.T.) ;
#5173 = EDGE_CURVE('',#4269,#4268,#2330,.T.) ;
#5174 = EDGE_CURVE('',#4253,#4269,#3821,.T.) ;
#5175 = EDGE_CURVE('',#4252,#4251,#3822,.T.) ;
#5176 = EDGE_CURVE('',#4270,#4250,#3823,.T.) ;
#5177 = EDGE_CURVE('',#4271,#4270,#2331,.T.) ;
#5178 = EDGE_CURVE('',#4271,#4267,#3824,.T.) ;
#5179 = EDGE_CURVE('',#4268,#4271,#2332,.T.) ;
#5180 = EDGE_CURVE('',#4272,#4270,#2333,.T.) ;
#5181 = EDGE_CURVE('',#4272,#4273,#2334,.T.) ;
#5182 = EDGE_CURVE('',#4273,#4274,#2335,.T.) ;
#5183 = EDGE_CURVE('',#4274,#4275,#2336,.T.) ;
#5184 = EDGE_CURVE('',#4276,#4275,#2337,.T.) ;
#5185 = EDGE_CURVE('',#4277,#4276,#2338,.T.) ;
#5186 = EDGE_CURVE('',#4277,#4278,#2339,.T.) ;
#5187 = EDGE_CURVE('',#4278,#4279,#2340,.T.) ;
#5188 = EDGE_CURVE('',#4279,#4280,#2341,.T.) ;
#5189 = EDGE_CURVE('',#4281,#4280,#2342,.T.) ;
#5190 = EDGE_CURVE('',#4269,#4281,#2343,.T.) ;
#5191 = EDGE_CURVE('',#4236,#4282,#2344,.T.) ;
#5192 = EDGE_CURVE('',#4282,#4283,#2345,.T.) ;
#5193 = EDGE_CURVE('',#4283,#4237,#2346,.T.) ;
#5194 = EDGE_CURVE('',#4231,#4284,#2347,.T.) ;
#5195 = EDGE_CURVE('',#4284,#4285,#2348,.T.) ;
#5196 = EDGE_CURVE('',#4285,#4232,#2349,.T.) ;
#5197 = EDGE_CURVE('',#4249,#4272,#3825,.T.) ;
#5198 = EDGE_CURVE('',#4285,#4229,#2350,.T.) ;
#5199 = EDGE_CURVE('',#4286,#4284,#2351,.T.) ;
#5200 = EDGE_CURVE('',#4286,#4230,#2352,.T.) ;
#5201 = EDGE_CURVE('',#4225,#4286,#3826,.T.) ;
#5202 = EDGE_CURVE('',#4287,#4288,#2353,.T.) ;
#5203 = EDGE_CURVE('',#4289,#4287,#2354,.T.) ;
#5204 = EDGE_CURVE('',#4289,#4290,#2355,.T.) ;
#5205 = EDGE_CURVE('',#4290,#4288,#2356,.T.) ;
#5206 = EDGE_CURVE('',#4288,#4291,#2357,.T.) ;
#5207 = EDGE_CURVE('',#4292,#4290,#2358,.T.) ;
#5208 = EDGE_CURVE('',#4292,#4291,#2359,.T.) ;
#5209 = EDGE_CURVE('',#4293,#4292,#2360,.T.) ;
#5210 = EDGE_CURVE('',#4293,#4289,#2361,.T.) ;
#5211 = EDGE_CURVE('',#4294,#4294,#3827,.T.) ;
#5212 = EDGE_CURVE('',#4294,#4295,#2362,.T.) ;
#5213 = EDGE_CURVE('',#4295,#4273,#3828,.T.) ;
#5214 = EDGE_CURVE('',#4248,#4247,#3829,.T.) ;
#5215 = EDGE_CURVE('',#4275,#4246,#3830,.T.) ;
#5216 = EDGE_CURVE('',#4274,#4295,#3831,.T.) ;
#5217 = EDGE_CURVE('',#4283,#4234,#2363,.T.) ;
#5218 = EDGE_CURVE('',#4296,#4282,#2364,.T.) ;
#5219 = EDGE_CURVE('',#4296,#4235,#2365,.T.) ;
#5220 = EDGE_CURVE('',#4221,#4296,#3832,.T.) ;
#5221 = EDGE_CURVE('',#4297,#4298,#2366,.T.) ;
#5222 = EDGE_CURVE('',#4297,#4299,#2367,.T.) ;
#5223 = EDGE_CURVE('',#4299,#4300,#2368,.T.) ;
#5224 = EDGE_CURVE('',#4298,#4300,#2369,.T.) ;
#5225 = EDGE_CURVE('',#4301,#4297,#2370,.T.) ;
#5226 = EDGE_CURVE('',#4301,#4302,#2371,.T.) ;
#5227 = EDGE_CURVE('',#4302,#4299,#2372,.T.) ;
#5228 = EDGE_CURVE('',#4302,#4303,#2373,.T.) ;
#5229 = EDGE_CURVE('',#4300,#4303,#2374,.T.) ;
#5230 = EDGE_CURVE('',#4263,#4304,#2375,.T.) ;
#5231 = EDGE_CURVE('',#4304,#4305,#2376,.T.) ;
#5232 = EDGE_CURVE('',#4305,#4264,#2377,.T.) ;
#5233 = EDGE_CURVE('',#4152,#4306,#2378,.T.) ;
#5234 = EDGE_CURVE('',#4307,#4306,#2379,.T.) ;
#5235 = EDGE_CURVE('',#4154,#4307,#2380,.T.) ;
#5236 = EDGE_CURVE('',#4264,#4307,#2381,.T.) ;
#5237 = EDGE_CURVE('',#4155,#4305,#2382,.T.) ;
#5238 = EDGE_CURVE('',#4153,#4304,#2383,.T.) ;
#5239 = EDGE_CURVE('',#4244,#4308,#2384,.T.) ;
#5240 = EDGE_CURVE('',#4308,#4309,#2385,.T.) ;
#5241 = EDGE_CURVE('',#4309,#4245,#2386,.T.) ;
#5242 = EDGE_CURVE('',#4160,#4309,#2387,.T.) ;
#5243 = EDGE_CURVE('',#4162,#4308,#2388,.T.) ;
#5244 = EDGE_CURVE('',#4310,#4244,#2389,.T.) ;
#5245 = EDGE_CURVE('',#4163,#4310,#2390,.T.) ;
#5246 = EDGE_CURVE('',#4311,#4310,#2391,.T.) ;
#5247 = EDGE_CURVE('',#4161,#4311,#2392,.T.) ;
#5248 = EDGE_CURVE('',#4311,#4306,#2393,.T.) ;
#5249 = EDGE_CURVE('',#4243,#4312,#2394,.T.) ;
#5250 = EDGE_CURVE('',#4303,#4312,#2395,.T.) ;
#5251 = EDGE_CURVE('',#4291,#4301,#2396,.T.) ;
#5252 = EDGE_CURVE('',#4313,#4293,#2397,.T.) ;
#5253 = EDGE_CURVE('',#4313,#4265,#2398,.T.) ;
#5254 = EDGE_CURVE('',#4314,#4298,#2399,.T.) ;
#5255 = EDGE_CURVE('',#4315,#4314,#2400,.T.) ;
#5256 = EDGE_CURVE('',#4287,#4315,#2401,.T.) ;
#5257 = EDGE_CURVE('',#4312,#4277,#2402,.T.) ;
#5258 = EDGE_CURVE('',#4314,#4276,#2403,.T.) ;
#5259 = EDGE_CURVE('',#4265,#4316,#2404,.T.) ;
#5260 = EDGE_CURVE('',#4316,#4257,#2405,.T.) ;
#5261 = EDGE_CURVE('',#4176,#4317,#2406,.T.) ;
#5262 = EDGE_CURVE('',#4279,#4317,#2407,.T.) ;
#5263 = EDGE_CURVE('',#4258,#4279,#2408,.T.) ;
#5264 = EDGE_CURVE('',#4177,#4316,#2409,.T.) ;
#5265 = EDGE_CURVE('',#4317,#4313,#2410,.T.) ;
#5266 = EDGE_CURVE('',#4280,#4313,#2411,.T.) ;
#5267 = EDGE_CURVE('',#4278,#4259,#2412,.T.) ;
#5268 = EDGE_CURVE('',#4260,#4318,#2413,.T.) ;
#5269 = EDGE_CURVE('',#4318,#4243,#2414,.T.) ;
#5270 = EDGE_CURVE('',#4312,#4319,#2415,.T.) ;
#5271 = EDGE_CURVE('',#4319,#4278,#2416,.T.) ;
#5272 = EDGE_CURVE('',#4168,#4318,#2417,.T.) ;
#5273 = EDGE_CURVE('',#4169,#4319,#2418,.T.) ;
#5274 = EDGE_CURVE('',#4281,#4315,#2419,.T.) ;
#5275 = EDGE_CURVE('',#4239,#4261,#2420,.T.) ;
#5276 = EDGE_CURVE('',#4320,#4320,#3833,.T.) ;
#5277 = EDGE_CURVE('',#4320,#4321,#2421,.T.) ;
#5278 = EDGE_CURVE('',#4321,#4321,#3834,.T.) ;
#5279 = EDGE_CURVE('',#4322,#4322,#3835,.T.) ;
#5280 = EDGE_CURVE('',#4322,#4323,#2422,.T.) ;
#5281 = EDGE_CURVE('',#4323,#4323,#3836,.T.) ;
#5282 = EDGE_CURVE('',#4324,#4325,#2423,.T.) ;
#5283 = EDGE_CURVE('',#4324,#4326,#2424,.T.) ;
#5284 = EDGE_CURVE('',#4326,#4327,#2425,.T.) ;
#5285 = EDGE_CURVE('',#4327,#4325,#2426,.T.) ;
#5286 = EDGE_CURVE('',#4328,#4324,#2427,.T.) ;
#5287 = EDGE_CURVE('',#4329,#4328,#2428,.T.) ;
#5288 = EDGE_CURVE('',#4330,#4329,#2429,.T.) ;
#5289 = EDGE_CURVE('',#4331,#4330,#2430,.T.) ;
#5290 = EDGE_CURVE('',#4331,#4326,#2431,.T.) ;
#5291 = EDGE_CURVE('',#4325,#4332,#2432,.T.) ;
#5292 = EDGE_CURVE('',#4333,#4327,#2433,.T.) ;
#5293 = EDGE_CURVE('',#4332,#4333,#2434,.T.) ;
#5294 = EDGE_CURVE('',#4333,#4331,#2435,.T.) ;
#5295 = EDGE_CURVE('',#4332,#4334,#2436,.T.) ;
#5296 = EDGE_CURVE('',#4335,#4330,#2437,.T.) ;
#5297 = EDGE_CURVE('',#4334,#4335,#2438,.T.) ;
#5298 = EDGE_CURVE('',#4328,#4336,#3837,.T.) ;
#5299 = EDGE_CURVE('',#4337,#4336,#2439,.T.) ;
#5300 = EDGE_CURVE('',#4329,#4337,#3838,.T.) ;
#5301 = EDGE_CURVE('',#4338,#4335,#3839,.T.) ;
#5302 = EDGE_CURVE('',#4338,#4339,#2440,.T.) ;
#5303 = EDGE_CURVE('',#4339,#4334,#3840,.T.) ;
#5304 = EDGE_CURVE('',#4340,#4341,#3841,.T.) ;
#5305 = EDGE_CURVE('',#4342,#4340,#2441,.T.) ;
#5306 = EDGE_CURVE('',#4343,#4342,#3842,.T.) ;
#5307 = EDGE_CURVE('',#4344,#4343,#2442,.T.) ;
#5308 = EDGE_CURVE('',#4345,#4344,#3843,.T.) ;
#5309 = EDGE_CURVE('',#4346,#4345,#2443,.T.) ;
#5310 = EDGE_CURVE('',#4347,#4346,#3844,.T.) ;
#5311 = EDGE_CURVE('',#4341,#4347,#2444,.T.) ;
#5312 = EDGE_CURVE('',#4337,#4348,#2445,.T.) ;
#5313 = EDGE_CURVE('',#4348,#4349,#3845,.T.) ;
#5314 = EDGE_CURVE('',#4349,#4350,#2446,.T.) ;
#5315 = EDGE_CURVE('',#4350,#4351,#2447,.T.) ;
#5316 = EDGE_CURVE('',#4351,#4352,#3846,.T.) ;
#5317 = EDGE_CURVE('',#4352,#4353,#2448,.T.) ;
#5318 = EDGE_CURVE('',#4353,#4354,#3847,.T.) ;
#5319 = EDGE_CURVE('',#4354,#4355,#2449,.T.) ;
#5320 = EDGE_CURVE('',#4355,#4356,#3848,.T.) ;
#5321 = EDGE_CURVE('',#4356,#4338,#2450,.T.) ;
#5322 = EDGE_CURVE('',#4357,#4358,#2451,.T.) ;
#5323 = EDGE_CURVE('',#4357,#4359,#2452,.T.) ;
#5324 = EDGE_CURVE('',#4359,#4360,#2453,.T.) ;
#5325 = EDGE_CURVE('',#4360,#4358,#2454,.T.) ;
#5326 = EDGE_CURVE('',#4361,#4357,#2455,.T.) ;
#5327 = EDGE_CURVE('',#4362,#4361,#2456,.T.) ;
#5328 = EDGE_CURVE('',#4359,#4362,#2457,.T.) ;
#5329 = EDGE_CURVE('',#4363,#4361,#2458,.T.) ;
#5330 = EDGE_CURVE('',#4351,#4363,#2459,.T.) ;
#5331 = EDGE_CURVE('',#4350,#4364,#2460,.T.) ;
#5332 = EDGE_CURVE('',#4364,#4362,#2461,.T.) ;
#5333 = EDGE_CURVE('',#4360,#4364,#2462,.T.) ;
#5334 = EDGE_CURVE('',#4358,#4365,#2463,.T.) ;
#5335 = EDGE_CURVE('',#4365,#4349,#2464,.T.) ;
#5336 = EDGE_CURVE('',#4363,#4366,#3849,.T.) ;
#5337 = EDGE_CURVE('',#4352,#4366,#2465,.T.) ;
#5338 = EDGE_CURVE('',#4348,#4367,#2466,.T.) ;
#5339 = EDGE_CURVE('',#4367,#4365,#3850,.T.) ;
#5340 = EDGE_CURVE('',#4368,#4369,#3851,.T.) ;
#5341 = EDGE_CURVE('',#4369,#4370,#2467,.T.) ;
#5342 = EDGE_CURVE('',#4370,#4371,#3852,.T.) ;
#5343 = EDGE_CURVE('',#4371,#4368,#2468,.T.) ;
#5344 = EDGE_CURVE('',#4372,#4373,#3853,.T.) ;
#5345 = EDGE_CURVE('',#4373,#4371,#3854,.T.) ;
#5346 = EDGE_CURVE('',#4370,#4372,#3855,.T.) ;
#5347 = EDGE_CURVE('',#4374,#4375,#3856,.T.) ;
#5348 = EDGE_CURVE('',#4375,#4373,#2469,.T.) ;
#5349 = EDGE_CURVE('',#4372,#4374,#2470,.T.) ;
#5350 = EDGE_CURVE('',#4376,#4377,#3857,.T.) ;
#5351 = EDGE_CURVE('',#4377,#4375,#3858,.T.) ;
#5352 = EDGE_CURVE('',#4374,#4376,#3859,.T.) ;
#5353 = EDGE_CURVE('',#4378,#4379,#3860,.T.) ;
#5354 = EDGE_CURVE('',#4379,#4377,#2471,.T.) ;
#5355 = EDGE_CURVE('',#4376,#4378,#2472,.T.) ;
#5356 = EDGE_CURVE('',#4380,#4381,#3861,.T.) ;
#5357 = EDGE_CURVE('',#4381,#4379,#3862,.T.) ;
#5358 = EDGE_CURVE('',#4378,#4380,#3863,.T.) ;
#5359 = EDGE_CURVE('',#4382,#4383,#3864,.T.) ;
#5360 = EDGE_CURVE('',#4383,#4381,#2473,.T.) ;
#5361 = EDGE_CURVE('',#4380,#4382,#2474,.T.) ;
#5362 = EDGE_CURVE('',#4368,#4383,#3865,.T.) ;
#5363 = EDGE_CURVE('',#4382,#4369,#3866,.T.) ;
#5364 = EDGE_CURVE('',#4347,#4374,#2475,.T.) ;
#5365 = EDGE_CURVE('',#4346,#4376,#2476,.T.) ;
#5366 = EDGE_CURVE('',#4341,#4372,#2477,.T.) ;
#5367 = EDGE_CURVE('',#4340,#4370,#2478,.T.) ;
#5368 = EDGE_CURVE('',#4342,#4369,#2479,.T.) ;
#5369 = EDGE_CURVE('',#4354,#4384,#2480,.T.) ;
#5370 = EDGE_CURVE('',#4384,#4385,#2481,.T.) ;
#5371 = EDGE_CURVE('',#4355,#4385,#2482,.T.) ;
#5372 = EDGE_CURVE('',#4353,#4386,#2483,.T.) ;
#5373 = EDGE_CURVE('',#4386,#4384,#3867,.T.) ;
#5374 = EDGE_CURVE('',#4366,#4386,#2484,.T.) ;
#5375 = EDGE_CURVE('',#4336,#4367,#2485,.T.) ;
#5376 = EDGE_CURVE('',#4356,#4387,#2486,.T.) ;
#5377 = EDGE_CURVE('',#4387,#4339,#2487,.T.) ;
#5378 = EDGE_CURVE('',#4385,#4387,#3868,.T.) ;
#5379 = EDGE_CURVE('',#4343,#4382,#2488,.T.) ;
#5380 = EDGE_CURVE('',#4344,#4380,#2489,.T.) ;
#5381 = EDGE_CURVE('',#4345,#4378,#2490,.T.) ;
#5382 = EDGE_CURVE('',#4388,#4388,#3869,.T.) ;
#5383 = EDGE_CURVE('',#4388,#4389,#2491,.T.) ;
#5384 = EDGE_CURVE('',#4389,#4389,#3870,.T.) ;
#5385 = EDGE_CURVE('',#4390,#4390,#3871,.T.) ;
#5386 = EDGE_CURVE('',#4390,#4391,#2492,.T.) ;
#5387 = EDGE_CURVE('',#4391,#4391,#3872,.T.) ;
#5388 = EDGE_CURVE('',#4392,#4392,#3873,.T.) ;
#5389 = EDGE_CURVE('',#4392,#4393,#2493,.T.) ;
#5390 = EDGE_CURVE('',#4393,#4393,#3874,.T.) ;
#5391 = EDGE_CURVE('',#4394,#4394,#3875,.T.) ;
#5392 = EDGE_CURVE('',#4394,#4395,#2494,.T.) ;
#5393 = EDGE_CURVE('',#4395,#4395,#3876,.T.) ;
#5394 = EDGE_CURVE('',#4396,#4397,#2495,.T.) ;
#5395 = EDGE_CURVE('',#4397,#4398,#2496,.T.) ;
#5396 = EDGE_CURVE('',#4399,#4398,#2497,.T.) ;
#5397 = EDGE_CURVE('',#4396,#4399,#2498,.T.) ;
#5398 = EDGE_CURVE('',#4400,#4396,#3877,.T.) ;
#5399 = EDGE_CURVE('',#4401,#4399,#3878,.T.) ;
#5400 = EDGE_CURVE('',#4400,#4401,#2499,.T.) ;
#5401 = EDGE_CURVE('',#4402,#4400,#2500,.T.) ;
#5402 = EDGE_CURVE('',#4403,#4401,#2501,.T.) ;
#5403 = EDGE_CURVE('',#4402,#4403,#2502,.T.) ;
#5404 = EDGE_CURVE('',#4397,#4402,#3879,.T.) ;
#5405 = EDGE_CURVE('',#4398,#4403,#3880,.T.) ;
#5406 = EDGE_CURVE('',#4404,#4404,#3881,.T.) ;
#5407 = EDGE_CURVE('',#4404,#4405,#2503,.T.) ;
#5408 = EDGE_CURVE('',#4405,#4405,#3882,.T.) ;
#5409 = EDGE_CURVE('',#4406,#4406,#3883,.T.) ;
#5410 = EDGE_CURVE('',#4406,#4407,#2504,.T.) ;
#5411 = EDGE_CURVE('',#4407,#4407,#3884,.T.) ;
#5412 = EDGE_CURVE('',#4408,#4408,#3885,.T.) ;
#5413 = EDGE_CURVE('',#4408,#4409,#2505,.T.) ;
#5414 = EDGE_CURVE('',#4409,#4409,#3886,.T.) ;
#5415 = EDGE_CURVE('',#4410,#4411,#2506,.T.) ;
#5416 = EDGE_CURVE('',#4411,#4412,#2507,.T.) ;
#5417 = EDGE_CURVE('',#4413,#4412,#2508,.T.) ;
#5418 = EDGE_CURVE('',#4410,#4413,#2509,.T.) ;
#5419 = EDGE_CURVE('',#4414,#4410,#3887,.T.) ;
#5420 = EDGE_CURVE('',#4415,#4413,#3888,.T.) ;
#5421 = EDGE_CURVE('',#4414,#4415,#2510,.T.) ;
#5422 = EDGE_CURVE('',#4416,#4414,#2511,.T.) ;
#5423 = EDGE_CURVE('',#4417,#4415,#2512,.T.) ;
#5424 = EDGE_CURVE('',#4416,#4417,#2513,.T.) ;
#5425 = EDGE_CURVE('',#4411,#4416,#3889,.T.) ;
#5426 = EDGE_CURVE('',#4412,#4417,#3890,.T.) ;
#5427 = EDGE_CURVE('',#4418,#4418,#3891,.T.) ;
#5428 = EDGE_CURVE('',#4418,#4419,#2514,.T.) ;
#5429 = EDGE_CURVE('',#4419,#4419,#3892,.T.) ;
#5430 = EDGE_CURVE('',#4420,#4420,#3893,.T.) ;
#5431 = EDGE_CURVE('',#4420,#4421,#2515,.T.) ;
#5432 = EDGE_CURVE('',#4421,#4421,#3894,.T.) ;
#5433 = EDGE_CURVE('',#4422,#4422,#3895,.T.) ;
#5434 = EDGE_CURVE('',#4422,#4423,#2516,.T.) ;
#5435 = EDGE_CURVE('',#4423,#4423,#3896,.T.) ;
#5436 = EDGE_CURVE('',#4424,#4424,#3897,.T.) ;
#5437 = EDGE_CURVE('',#4424,#4425,#2517,.T.) ;
#5438 = EDGE_CURVE('',#4425,#4425,#3898,.T.) ;
#5439 = EDGE_CURVE('',#4426,#4426,#3899,.T.) ;
#5440 = EDGE_CURVE('',#4426,#4427,#2518,.T.) ;
#5441 = EDGE_CURVE('',#4427,#4427,#3900,.T.) ;
#5442 = EDGE_CURVE('',#4428,#4429,#2519,.T.) ;
#5443 = EDGE_CURVE('',#4429,#4430,#2520,.T.) ;
#5444 = EDGE_CURVE('',#4431,#4430,#2521,.T.) ;
#5445 = EDGE_CURVE('',#4428,#4431,#2522,.T.) ;
#5446 = EDGE_CURVE('',#4432,#4428,#3901,.T.) ;
#5447 = EDGE_CURVE('',#4433,#4431,#3902,.T.) ;
#5448 = EDGE_CURVE('',#4432,#4433,#2523,.T.) ;
#5449 = EDGE_CURVE('',#4434,#4432,#2524,.T.) ;
#5450 = EDGE_CURVE('',#4435,#4433,#2525,.T.) ;
#5451 = EDGE_CURVE('',#4434,#4435,#2526,.T.) ;
#5452 = EDGE_CURVE('',#4429,#4434,#3903,.T.) ;
#5453 = EDGE_CURVE('',#4430,#4435,#3904,.T.) ;
#5454 = EDGE_CURVE('',#4436,#4436,#3905,.T.) ;
#5455 = EDGE_CURVE('',#4436,#4437,#2527,.T.) ;
#5456 = EDGE_CURVE('',#4437,#4437,#3906,.T.) ;
#5457 = EDGE_CURVE('',#4438,#4438,#3907,.T.) ;
#5458 = EDGE_CURVE('',#4438,#4439,#2528,.T.) ;
#5459 = EDGE_CURVE('',#4439,#4439,#3908,.T.) ;
#5460 = EDGE_CURVE('',#4440,#4440,#3909,.T.) ;
#5461 = EDGE_CURVE('',#4440,#4441,#2529,.T.) ;
#5462 = EDGE_CURVE('',#4441,#4441,#3910,.T.) ;
#5463 = EDGE_CURVE('',#4442,#4443,#2530,.T.) ;
#5464 = EDGE_CURVE('',#4443,#4444,#2531,.T.) ;
#5465 = EDGE_CURVE('',#4445,#4444,#2532,.T.) ;
#5466 = EDGE_CURVE('',#4442,#4445,#2533,.T.) ;
#5467 = EDGE_CURVE('',#4446,#4442,#3911,.T.) ;
#5468 = EDGE_CURVE('',#4447,#4445,#3912,.T.) ;
#5469 = EDGE_CURVE('',#4446,#4447,#2534,.T.) ;
#5470 = EDGE_CURVE('',#4448,#4446,#2535,.T.) ;
#5471 = EDGE_CURVE('',#4449,#4447,#2536,.T.) ;
#5472 = EDGE_CURVE('',#4448,#4449,#2537,.T.) ;
#5473 = EDGE_CURVE('',#4443,#4448,#3913,.T.) ;
#5474 = EDGE_CURVE('',#4444,#4449,#3914,.T.) ;
#5475 = EDGE_CURVE('',#4450,#4451,#2538,.T.) ;
#5476 = EDGE_CURVE('',#4451,#4452,#3915,.T.) ;
#5477 = EDGE_CURVE('',#4452,#4450,#419,.T.) ;
#5478 = EDGE_CURVE('',#4453,#4454,#2539,.T.) ;
#5479 = EDGE_CURVE('',#4455,#4453,#3916,.T.) ;
#5480 = EDGE_CURVE('',#4455,#4456,#420,.T.) ;
#5481 = EDGE_CURVE('',#4456,#4452,#421,.T.) ;
#5482 = EDGE_CURVE('',#4452,#4451,#3917,.T.) ;
#5483 = EDGE_CURVE('',#4450,#4454,#422,.T.) ;
#5484 = EDGE_CURVE('',#4457,#4457,#3918,.T.) ;
#5485 = EDGE_CURVE('',#4457,#4458,#2540,.T.) ;
#5486 = EDGE_CURVE('',#4458,#4458,#3919,.T.) ;
#5487 = EDGE_CURVE('',#4459,#4459,#3920,.T.) ;
#5488 = EDGE_CURVE('',#4459,#4460,#2541,.T.) ;
#5489 = EDGE_CURVE('',#4460,#4460,#3921,.T.) ;
#5490 = EDGE_CURVE('',#4461,#4461,#3922,.T.) ;
#5491 = EDGE_CURVE('',#4461,#4462,#2542,.T.) ;
#5492 = EDGE_CURVE('',#4462,#4462,#3923,.T.) ;
#5493 = EDGE_CURVE('',#4463,#4463,#3924,.T.) ;
#5494 = EDGE_CURVE('',#4464,#4464,#3925,.T.) ;
#5495 = EDGE_CURVE('',#4464,#4463,#2543,.T.) ;
#5496 = EDGE_CURVE('',#4465,#4465,#3926,.T.) ;
#5497 = EDGE_CURVE('',#4454,#4455,#423,.T.) ;
#5498 = EDGE_CURVE('',#4456,#4465,#2544,.T.) ;
#5499 = EDGE_CURVE('',#4453,#4455,#3927,.T.) ;
#5500 = EDGE_CURVE('',#4466,#4467,#2545,.T.) ;
#5501 = EDGE_CURVE('',#4468,#4466,#3928,.T.) ;
#5502 = EDGE_CURVE('',#4469,#4468,#424,.T.) ;
#5503 = EDGE_CURVE('',#4470,#4469,#2546,.T.) ;
#5504 = EDGE_CURVE('',#4471,#4470,#425,.T.) ;
#5505 = EDGE_CURVE('',#4471,#4467,#3929,.T.) ;
#5506 = EDGE_CURVE('',#4472,#4472,#3930,.T.) ;
#5507 = EDGE_CURVE('',#4472,#4473,#2547,.T.) ;
#5508 = EDGE_CURVE('',#4473,#4473,#3931,.T.) ;
#5509 = EDGE_CURVE('',#4467,#4471,#3932,.T.) ;
#5510 = EDGE_CURVE('',#4474,#4471,#426,.T.) ;
#5511 = EDGE_CURVE('',#4475,#4474,#2548,.T.) ;
#5512 = EDGE_CURVE('',#4468,#4475,#427,.T.) ;
#5513 = EDGE_CURVE('',#4466,#4468,#3933,.T.) ;
#5514 = EDGE_CURVE('',#4476,#4474,#3934,.T.) ;
#5515 = EDGE_CURVE('',#4475,#4476,#3935,.T.) ;
#5516 = EDGE_CURVE('',#4470,#4469,#3936,.T.) ;
#5517 = EDGE_CURVE('',#4477,#4477,#3937,.T.) ;
#5518 = EDGE_CURVE('',#4477,#4476,#2549,.T.) ;
#5519 = EDGE_CURVE('',#4478,#4478,#3938,.T.) ;
#5520 = EDGE_CURVE('',#4479,#4479,#3939,.T.) ;
#5521 = EDGE_CURVE('',#4479,#4478,#2550,.T.) ;
#5522 = EDGE_CURVE('',#4480,#4481,#2551,.T.) ;
#5523 = EDGE_CURVE('',#4482,#4480,#3940,.T.) ;
#5524 = EDGE_CURVE('',#4483,#4482,#2552,.T.) ;
#5525 = EDGE_CURVE('',#4481,#4483,#3941,.T.) ;
#5526 = EDGE_CURVE('',#4480,#4484,#2553,.T.) ;
#5527 = EDGE_CURVE('',#4484,#4485,#2554,.T.) ;
#5528 = EDGE_CURVE('',#4485,#4486,#2555,.T.) ;
#5529 = EDGE_CURVE('',#4487,#4486,#2556,.T.) ;
#5530 = EDGE_CURVE('',#4488,#4487,#245,.T.) ;
#5531 = EDGE_CURVE('',#4489,#4488,#2557,.T.) ;
#5532 = EDGE_CURVE('',#4489,#4490,#2558,.T.) ;
#5533 = EDGE_CURVE('',#4490,#4482,#2559,.T.) ;
#5534 = EDGE_CURVE('',#4491,#4481,#2560,.T.) ;
#5535 = EDGE_CURVE('',#4484,#4491,#2561,.T.) ;
#5536 = EDGE_CURVE('',#4490,#4492,#2562,.T.) ;
#5537 = EDGE_CURVE('',#4483,#4492,#2563,.T.) ;
#5538 = EDGE_CURVE('',#4493,#4494,#3942,.T.) ;
#5539 = EDGE_CURVE('',#4493,#4495,#2564,.T.) ;
#5540 = EDGE_CURVE('',#4494,#4495,#2565,.T.) ;
#5541 = EDGE_CURVE('',#4494,#4489,#3943,.T.) ;
#5542 = EDGE_CURVE('',#4492,#4494,#2566,.T.) ;
#5543 = EDGE_CURVE('',#4486,#4496,#2567,.T.) ;
#5544 = EDGE_CURVE('',#4485,#4497,#2568,.T.) ;
#5545 = EDGE_CURVE('',#4495,#4497,#2569,.T.) ;
#5546 = EDGE_CURVE('',#4498,#4493,#2570,.T.) ;
#5547 = EDGE_CURVE('',#4496,#4498,#246,.T.) ;
#5548 = EDGE_CURVE('',#4497,#4491,#2571,.T.) ;
#5549 = EDGE_CURVE('',#4496,#4487,#3944,.T.) ;
#5550 = EDGE_CURVE('',#4498,#4499,#3945,.T.) ;
#5551 = EDGE_CURVE('',#4499,#4488,#3946,.T.) ;
#5552 = EDGE_CURVE('',#4500,#4501,#2572,.T.) ;
#5553 = EDGE_CURVE('',#4501,#4500,#3947,.T.) ;
#5554 = EDGE_CURVE('',#4499,#4502,#2573,.T.) ;
#5555 = EDGE_CURVE('',#4503,#4502,#3948,.T.) ;
#5556 = EDGE_CURVE('',#4501,#4503,#2574,.T.) ;
#5557 = EDGE_CURVE('',#4504,#4500,#2575,.T.) ;
#5558 = EDGE_CURVE('',#4502,#4504,#3949,.T.) ;
#5559 = EDGE_CURVE('',#4504,#4505,#2576,.T.) ;
#5560 = EDGE_CURVE('',#4505,#4506,#2577,.T.) ;
#5561 = EDGE_CURVE('',#4506,#4507,#2578,.T.) ;
#5562 = EDGE_CURVE('',#4507,#4508,#2579,.T.) ;
#5563 = EDGE_CURVE('',#4508,#4503,#2580,.T.) ;
#5564 = EDGE_CURVE('',#4509,#4510,#2581,.T.) ;
#5565 = EDGE_CURVE('',#4510,#4506,#2582,.T.) ;
#5566 = EDGE_CURVE('',#4509,#4505,#2583,.T.) ;
#5567 = EDGE_CURVE('',#4511,#4508,#2584,.T.) ;
#5568 = EDGE_CURVE('',#4511,#4509,#2585,.T.) ;
#5569 = EDGE_CURVE('',#4512,#4511,#2586,.T.) ;
#5570 = EDGE_CURVE('',#4512,#4507,#2587,.T.) ;
#5571 = EDGE_CURVE('',#4510,#4512,#2588,.T.) ;
#5572 = EDGE_CURVE('',#4513,#4514,#2589,.T.) ;
#5573 = EDGE_CURVE('',#4514,#4515,#2590,.T.) ;
#5574 = EDGE_CURVE('',#4516,#4515,#2591,.T.) ;
#5575 = EDGE_CURVE('',#4513,#4516,#2592,.T.) ;
#5576 = EDGE_CURVE('',#4517,#4513,#2593,.T.) ;
#5577 = EDGE_CURVE('',#4518,#4516,#2594,.T.) ;
#5578 = EDGE_CURVE('',#4517,#4518,#2595,.T.) ;
#5579 = EDGE_CURVE('',#4514,#4519,#2596,.T.) ;
#5580 = EDGE_CURVE('',#4519,#4520,#2597,.T.) ;
#5581 = EDGE_CURVE('',#4515,#4520,#2598,.T.) ;
#5582 = EDGE_CURVE('',#4521,#4522,#2599,.T.) ;
#5583 = EDGE_CURVE('',#4521,#4518,#2600,.T.) ;
#5584 = EDGE_CURVE('',#4520,#4523,#2601,.T.) ;
#5585 = EDGE_CURVE('',#4524,#4523,#2602,.T.) ;
#5586 = EDGE_CURVE('',#4522,#4524,#2603,.T.) ;
#5587 = EDGE_CURVE('',#4519,#4517,#2604,.T.) ;
#5588 = EDGE_CURVE('',#4524,#4525,#2605,.T.) ;
#5589 = EDGE_CURVE('',#4525,#4526,#3950,.T.) ;
#5590 = EDGE_CURVE('',#4526,#4527,#2606,.T.) ;
#5591 = EDGE_CURVE('',#4527,#4522,#3951,.T.) ;
#5592 = EDGE_CURVE('',#4528,#4528,#3952,.T.) ;
#5593 = EDGE_CURVE('',#4523,#4529,#2607,.T.) ;
#5594 = EDGE_CURVE('',#4529,#4525,#2608,.T.) ;
#5595 = EDGE_CURVE('',#4528,#4530,#2609,.T.) ;
#5596 = EDGE_CURVE('',#4530,#4530,#3953,.T.) ;
#5597 = EDGE_CURVE('',#4531,#4527,#2610,.T.) ;
#5598 = EDGE_CURVE('',#4531,#4521,#3954,.T.) ;
#5599 = EDGE_CURVE('',#4532,#4531,#2611,.T.) ;
#5600 = EDGE_CURVE('',#4532,#4526,#2612,.T.) ;
#5601 = EDGE_CURVE('',#4529,#4532,#3955,.T.) ;
#5602 = EDGE_CURVE('',#4533,#4534,#428,.T.) ;
#5603 = EDGE_CURVE('',#4534,#4533,#429,.T.) ;
#5604 = EDGE_CURVE('',#4534,#4535,#2613,.T.) ;
#5605 = EDGE_CURVE('',#4536,#4535,#430,.T.) ;
#5606 = EDGE_CURVE('',#4535,#4536,#431,.T.) ;
#5607 = EDGE_CURVE('',#4537,#4538,#432,.T.) ;
#5608 = EDGE_CURVE('',#4537,#4539,#2614,.T.) ;
#5609 = EDGE_CURVE('',#4540,#4539,#433,.T.) ;
#5610 = EDGE_CURVE('',#4539,#4540,#434,.T.) ;
#5611 = EDGE_CURVE('',#4538,#4537,#435,.T.) ;
#5612 = EDGE_CURVE('',#4541,#4541,#3956,.T.) ;
#5613 = EDGE_CURVE('',#4541,#4542,#2615,.T.) ;
#5614 = EDGE_CURVE('',#4542,#4542,#3957,.T.) ;
#5615 = EDGE_CURVE('',#4543,#4544,#3958,.T.) ;
#5616 = EDGE_CURVE('',#4543,#4545,#2616,.T.) ;
#5617 = EDGE_CURVE('',#4545,#4546,#2617,.T.) ;
#5618 = EDGE_CURVE('',#4546,#4547,#2618,.T.) ;
#5619 = EDGE_CURVE('',#4547,#4548,#2619,.T.) ;
#5620 = EDGE_CURVE('',#4548,#4544,#2620,.T.) ;
#5621 = EDGE_CURVE('',#4549,#4543,#2621,.T.) ;
#5622 = EDGE_CURVE('',#4549,#4550,#2622,.T.) ;
#5623 = EDGE_CURVE('',#4550,#4545,#2623,.T.) ;
#5624 = EDGE_CURVE('',#4551,#4552,#2624,.T.) ;
#5625 = EDGE_CURVE('',#4552,#4548,#2625,.T.) ;
#5626 = EDGE_CURVE('',#4551,#4547,#2626,.T.) ;
#5627 = EDGE_CURVE('',#4553,#4551,#2627,.T.) ;
#5628 = EDGE_CURVE('',#4553,#4546,#2628,.T.) ;
#5629 = EDGE_CURVE('',#4550,#4553,#2629,.T.) ;
#5630 = EDGE_CURVE('',#4544,#4554,#2630,.T.) ;
#5631 = EDGE_CURVE('',#4552,#4554,#2631,.T.) ;
#5632 = EDGE_CURVE('',#4554,#4549,#3959,.T.) ;
#5633 = EDGE_CURVE('',#4555,#4555,#3960,.T.) ;
#5634 = EDGE_CURVE('',#4555,#4536,#2632,.T.) ;
#5635 = EDGE_CURVE('',#4535,#4556,#2633,.T.) ;
#5636 = EDGE_CURVE('',#4556,#4557,#3961,.T.) ;
#5637 = EDGE_CURVE('',#4557,#4556,#3962,.T.) ;
#5638 = EDGE_CURVE('',#4557,#4558,#3963,.T.) ;
#5639 = EDGE_CURVE('',#4558,#4559,#3964,.T.) ;
#5640 = EDGE_CURVE('',#4559,#4558,#3965,.T.) ;
#5641 = EDGE_CURVE('',#4559,#4560,#2634,.T.) ;
#5642 = EDGE_CURVE('',#4560,#4561,#3966,.T.) ;
#5643 = EDGE_CURVE('',#4561,#4560,#3967,.T.) ;
#5644 = EDGE_CURVE('',#4561,#4562,#3968,.T.) ;
#5645 = EDGE_CURVE('',#4562,#4563,#3969,.T.) ;
#5646 = EDGE_CURVE('',#4563,#4562,#3970,.T.) ;
#5647 = EDGE_CURVE('',#4563,#4539,#2635,.T.) ;
#5648 = EDGE_CURVE('',#4540,#4564,#2636,.T.) ;
#5649 = EDGE_CURVE('',#4564,#4564,#3971,.T.) ;
#5650 = EDGE_CURVE('',#4565,#4565,#3972,.T.) ;
#5651 = EDGE_CURVE('',#4565,#4566,#2637,.T.) ;
#5652 = EDGE_CURVE('',#4566,#4566,#3973,.T.) ;
#5653 = EDGE_CURVE('',#4567,#4568,#2638,.T.) ;
#5654 = EDGE_CURVE('',#4568,#4569,#2639,.T.) ;
#5655 = EDGE_CURVE('',#4570,#4569,#2640,.T.) ;
#5656 = EDGE_CURVE('',#4567,#4570,#2641,.T.) ;
#5657 = EDGE_CURVE('',#4571,#4567,#3974,.T.) ;
#5658 = EDGE_CURVE('',#4572,#4570,#3975,.T.) ;
#5659 = EDGE_CURVE('',#4571,#4572,#2642,.T.) ;
#5660 = EDGE_CURVE('',#4573,#4571,#2643,.T.) ;
#5661 = EDGE_CURVE('',#4574,#4572,#2644,.T.) ;
#5662 = EDGE_CURVE('',#4573,#4574,#2645,.T.) ;
#5663 = EDGE_CURVE('',#4568,#4573,#3976,.T.) ;
#5664 = EDGE_CURVE('',#4569,#4574,#3977,.T.) ;
#5665 = EDGE_CURVE('',#4575,#4575,#3978,.T.) ;
#5666 = EDGE_CURVE('',#4576,#4576,#3979,.T.) ;
#5667 = EDGE_CURVE('',#4576,#4575,#2646,.T.) ;
#5668 = EDGE_CURVE('',#4577,#4577,#3980,.T.) ;
#5669 = EDGE_CURVE('',#4577,#4576,#2647,.T.) ;
#5670 = EDGE_CURVE('',#4578,#4578,#3981,.T.) ;
#5671 = EDGE_CURVE('',#4579,#4579,#3982,.T.) ;
#5672 = EDGE_CURVE('',#4579,#4578,#2648,.T.) ;
#5673 = EDGE_CURVE('',#4580,#4580,#3983,.T.) ;
#5674 = EDGE_CURVE('',#4581,#4581,#3984,.T.) ;
#5675 = EDGE_CURVE('',#4581,#4580,#2649,.T.) ;
#5676 = EDGE_CURVE('',#4582,#4582,#3985,.T.) ;
#5677 = EDGE_CURVE('',#4583,#4583,#3986,.T.) ;
#5678 = EDGE_CURVE('',#4583,#4582,#2650,.T.) ;
#5679 = EDGE_CURVE('',#4584,#4584,#3987,.T.) ;
#5680 = EDGE_CURVE('',#4584,#4583,#2651,.T.) ;
#5681 = EDGE_CURVE('',#4585,#4586,#2652,.T.) ;
#5682 = EDGE_CURVE('',#4587,#4585,#2653,.T.) ;
#5683 = EDGE_CURVE('',#4588,#4587,#2654,.T.) ;
#5684 = EDGE_CURVE('',#4586,#4588,#2655,.T.) ;
#5685 = EDGE_CURVE('',#4589,#4590,#2656,.T.) ;
#5686 = EDGE_CURVE('',#4589,#4591,#2657,.T.) ;
#5687 = EDGE_CURVE('',#4592,#4591,#2658,.T.) ;
#5688 = EDGE_CURVE('',#4590,#4592,#2659,.T.) ;
#5689 = EDGE_CURVE('',#4586,#4593,#2660,.T.) ;
#5690 = EDGE_CURVE('',#4594,#4588,#2661,.T.) ;
#5691 = EDGE_CURVE('',#4593,#4594,#2662,.T.) ;
#5692 = EDGE_CURVE('',#4595,#4589,#2663,.T.) ;
#5693 = EDGE_CURVE('',#4596,#4595,#2664,.T.) ;
#5694 = EDGE_CURVE('',#4591,#4596,#2665,.T.) ;
#5695 = EDGE_CURVE('',#4587,#4592,#3988,.T.) ;
#5696 = EDGE_CURVE('',#4585,#4590,#3989,.T.) ;
#5697 = EDGE_CURVE('',#4594,#4596,#3990,.T.) ;
#5698 = EDGE_CURVE('',#4593,#4595,#3991,.T.) ;
#5699 = EDGE_CURVE('',#4597,#4597,#3992,.T.) ;
#5700 = EDGE_CURVE('',#4598,#4598,#3993,.T.) ;
#5701 = EDGE_CURVE('',#4598,#4597,#2666,.T.) ;
#5702 = EDGE_CURVE('',#4599,#4599,#3994,.T.) ;
#5703 = EDGE_CURVE('',#4599,#4598,#2667,.T.) ;
#5704 = EDGE_CURVE('',#4600,#4600,#3995,.T.) ;
#5705 = EDGE_CURVE('',#4600,#4599,#2668,.T.) ;
#5706 = EDGE_CURVE('',#4601,#4601,#3996,.T.) ;
#5707 = EDGE_CURVE('',#4602,#4602,#3997,.T.) ;
#5708 = EDGE_CURVE('',#4602,#4601,#2669,.T.) ;
#5709 = EDGE_CURVE('',#4603,#4603,#3998,.T.) ;
#5710 = EDGE_CURVE('',#4603,#4602,#2670,.T.) ;
#5711 = EDGE_CURVE('',#4604,#4605,#2671,.T.) ;
#5712 = EDGE_CURVE('',#4604,#4606,#436,.T.) ;
#5713 = EDGE_CURVE('',#4607,#4606,#3999,.T.) ;
#5714 = EDGE_CURVE('',#4607,#4605,#437,.T.) ;
#5715 = EDGE_CURVE('',#4608,#4609,#2672,.T.) ;
#5716 = EDGE_CURVE('',#4608,#4604,#438,.T.) ;
#5717 = EDGE_CURVE('',#4605,#4609,#439,.T.) ;
#5718 = EDGE_CURVE('',#4610,#4611,#2673,.T.) ;
#5719 = EDGE_CURVE('',#4610,#4608,#440,.T.) ;
#5720 = EDGE_CURVE('',#4609,#4611,#441,.T.) ;
#5721 = EDGE_CURVE('',#4612,#4613,#2674,.T.) ;
#5722 = EDGE_CURVE('',#4612,#4610,#442,.T.) ;
#5723 = EDGE_CURVE('',#4611,#4613,#443,.T.) ;
#5724 = EDGE_CURVE('',#4614,#4615,#2675,.T.) ;
#5725 = EDGE_CURVE('',#4614,#4612,#444,.T.) ;
#5726 = EDGE_CURVE('',#4613,#4615,#445,.T.) ;
#5727 = EDGE_CURVE('',#4616,#4617,#2676,.T.) ;
#5728 = EDGE_CURVE('',#4616,#4614,#446,.T.) ;
#5729 = EDGE_CURVE('',#4615,#4617,#447,.T.) ;
#5730 = EDGE_CURVE('',#4618,#4619,#2677,.T.) ;
#5731 = EDGE_CURVE('',#4618,#4616,#448,.T.) ;
#5732 = EDGE_CURVE('',#4617,#4619,#449,.T.) ;
#5733 = EDGE_CURVE('',#4620,#4621,#2678,.T.) ;
#5734 = EDGE_CURVE('',#4620,#4618,#450,.T.) ;
#5735 = EDGE_CURVE('',#4619,#4621,#451,.T.) ;
#5736 = EDGE_CURVE('',#4622,#4623,#2679,.T.) ;
#5737 = EDGE_CURVE('',#4622,#4620,#452,.T.) ;
#5738 = EDGE_CURVE('',#4621,#4623,#453,.T.) ;
#5739 = EDGE_CURVE('',#4624,#4625,#2680,.T.) ;
#5740 = EDGE_CURVE('',#4624,#4622,#454,.T.) ;
#5741 = EDGE_CURVE('',#4623,#4625,#455,.T.) ;
#5742 = EDGE_CURVE('',#4626,#4627,#2681,.T.) ;
#5743 = EDGE_CURVE('',#4626,#4624,#456,.T.) ;
#5744 = EDGE_CURVE('',#4625,#4627,#457,.T.) ;
#5745 = EDGE_CURVE('',#4628,#4629,#2682,.T.) ;
#5746 = EDGE_CURVE('',#4628,#4626,#458,.T.) ;
#5747 = EDGE_CURVE('',#4627,#4629,#459,.T.) ;
#5748 = EDGE_CURVE('',#4630,#4631,#2683,.T.) ;
#5749 = EDGE_CURVE('',#4630,#4628,#460,.T.) ;
#5750 = EDGE_CURVE('',#4629,#4631,#461,.T.) ;
#5751 = EDGE_CURVE('',#4632,#4633,#2684,.T.) ;
#5752 = EDGE_CURVE('',#4632,#4630,#462,.T.) ;
#5753 = EDGE_CURVE('',#4631,#4633,#463,.T.) ;
#5754 = EDGE_CURVE('',#4634,#4635,#2685,.T.) ;
#5755 = EDGE_CURVE('',#4634,#4636,#464,.T.) ;
#5756 = EDGE_CURVE('',#4637,#4636,#4000,.T.) ;
#5757 = EDGE_CURVE('',#4635,#4637,#465,.T.) ;
#5758 = EDGE_CURVE('',#4638,#4639,#2686,.T.) ;
#5759 = EDGE_CURVE('',#4638,#4634,#466,.T.) ;
#5760 = EDGE_CURVE('',#4639,#4635,#467,.T.) ;
#5761 = EDGE_CURVE('',#4640,#4641,#2687,.T.) ;
#5762 = EDGE_CURVE('',#4640,#4638,#468,.T.) ;
#5763 = EDGE_CURVE('',#4641,#4639,#469,.T.) ;
#5764 = EDGE_CURVE('',#4642,#4643,#2688,.T.) ;
#5765 = EDGE_CURVE('',#4642,#4640,#470,.T.) ;
#5766 = EDGE_CURVE('',#4643,#4641,#471,.T.) ;
#5767 = EDGE_CURVE('',#4644,#4645,#2689,.T.) ;
#5768 = EDGE_CURVE('',#4644,#4642,#472,.T.) ;
#5769 = EDGE_CURVE('',#4645,#4643,#473,.T.) ;
#5770 = EDGE_CURVE('',#4646,#4647,#2690,.T.) ;
#5771 = EDGE_CURVE('',#4646,#4644,#474,.T.) ;
#5772 = EDGE_CURVE('',#4647,#4645,#475,.T.) ;
#5773 = EDGE_CURVE('',#4648,#4649,#2691,.T.) ;
#5774 = EDGE_CURVE('',#4648,#4646,#476,.T.) ;
#5775 = EDGE_CURVE('',#4649,#4647,#477,.T.) ;
#5776 = EDGE_CURVE('',#4650,#4651,#2692,.T.) ;
#5777 = EDGE_CURVE('',#4650,#4648,#478,.T.) ;
#5778 = EDGE_CURVE('',#4651,#4649,#479,.T.) ;
#5779 = EDGE_CURVE('',#4652,#4653,#2693,.T.) ;
#5780 = EDGE_CURVE('',#4652,#4650,#480,.T.) ;
#5781 = EDGE_CURVE('',#4653,#4651,#481,.T.) ;
#5782 = EDGE_CURVE('',#4654,#4655,#2694,.T.) ;
#5783 = EDGE_CURVE('',#4654,#4652,#482,.T.) ;
#5784 = EDGE_CURVE('',#4655,#4653,#483,.T.) ;
#5785 = EDGE_CURVE('',#4656,#4657,#2695,.T.) ;
#5786 = EDGE_CURVE('',#4656,#4654,#484,.T.) ;
#5787 = EDGE_CURVE('',#4657,#4655,#485,.T.) ;
#5788 = EDGE_CURVE('',#4658,#4659,#2696,.T.) ;
#5789 = EDGE_CURVE('',#4658,#4656,#486,.T.) ;
#5790 = EDGE_CURVE('',#4659,#4657,#487,.T.) ;
#5791 = EDGE_CURVE('',#4660,#4661,#2697,.T.) ;
#5792 = EDGE_CURVE('',#4660,#4658,#488,.T.) ;
#5793 = EDGE_CURVE('',#4661,#4659,#489,.T.) ;
#5794 = EDGE_CURVE('',#4662,#4663,#2698,.T.) ;
#5795 = EDGE_CURVE('',#4662,#4660,#490,.T.) ;
#5796 = EDGE_CURVE('',#4663,#4661,#491,.T.) ;
#5797 = EDGE_CURVE('',#4636,#4664,#492,.T.) ;
#5798 = EDGE_CURVE('',#4665,#4664,#4001,.T.) ;
#5799 = EDGE_CURVE('',#4666,#4665,#4002,.T.) ;
#5800 = EDGE_CURVE('',#4666,#4637,#493,.T.) ;
#5801 = EDGE_CURVE('',#4633,#4666,#494,.T.) ;
#5802 = EDGE_CURVE('',#4667,#4607,#495,.T.) ;
#5803 = EDGE_CURVE('',#4667,#4663,#496,.T.) ;
#5804 = EDGE_CURVE('',#4606,#4668,#4003,.T.) ;
#5805 = EDGE_CURVE('',#4606,#4669,#497,.T.) ;
#5806 = EDGE_CURVE('',#4669,#4667,#4004,.T.) ;
#5807 = EDGE_CURVE('',#4668,#4607,#4005,.T.) ;
#5808 = EDGE_CURVE('',#4669,#4662,#498,.T.) ;
#5809 = EDGE_CURVE('',#4664,#4632,#499,.T.) ;
#5810 = EDGE_CURVE('',#4668,#4670,#4006,.T.) ;
#5811 = EDGE_CURVE('',#4670,#4670,#4007,.T.) ;
#5812 = EDGE_CURVE('',#4664,#4666,#4008,.T.) ;
#5813 = EDGE_CURVE('',#4671,#4671,#4009,.T.) ;
#5814 = EDGE_CURVE('',#4665,#4672,#2699,.T.) ;
#5815 = EDGE_CURVE('',#4672,#4672,#4010,.T.) ;
#5816 = EDGE_CURVE('',#4673,#4674,#4011,.T.) ;
#5817 = EDGE_CURVE('',#4675,#4673,#2700,.T.) ;
#5818 = EDGE_CURVE('',#4674,#4675,#2701,.T.) ;
#5819 = EDGE_CURVE('',#4674,#4676,#2702,.T.) ;
#5820 = EDGE_CURVE('',#4677,#4675,#2703,.T.) ;
#5821 = EDGE_CURVE('',#4676,#4677,#247,.T.) ;
#5822 = EDGE_CURVE('',#4678,#4673,#2704,.T.) ;
#5823 = EDGE_CURVE('',#4677,#4678,#248,.T.) ;
#5824 = EDGE_CURVE('',#4679,#4676,#4012,.T.) ;
#5825 = EDGE_CURVE('',#4679,#4680,#2705,.T.) ;
#5826 = EDGE_CURVE('',#4680,#4681,#4013,.T.) ;
#5827 = EDGE_CURVE('',#4681,#4682,#2706,.T.) ;
#5828 = EDGE_CURVE('',#4683,#4682,#4014,.T.) ;
#5829 = EDGE_CURVE('',#4683,#4684,#2707,.T.) ;
#5830 = EDGE_CURVE('',#4684,#4685,#4015,.T.) ;
#5831 = EDGE_CURVE('',#4685,#4686,#2708,.T.) ;
#5832 = EDGE_CURVE('',#4687,#4686,#4016,.T.) ;
#5833 = EDGE_CURVE('',#4687,#4688,#2709,.T.) ;
#5834 = EDGE_CURVE('',#4688,#4689,#4017,.T.) ;
#5835 = EDGE_CURVE('',#4689,#4690,#2710,.T.) ;
#5836 = EDGE_CURVE('',#4691,#4690,#4018,.T.) ;
#5837 = EDGE_CURVE('',#4691,#4692,#2711,.T.) ;
#5838 = EDGE_CURVE('',#4692,#4693,#4019,.T.) ;
#5839 = EDGE_CURVE('',#4693,#4694,#2712,.T.) ;
#5840 = EDGE_CURVE('',#4695,#4694,#4020,.T.) ;
#5841 = EDGE_CURVE('',#4695,#4696,#2713,.T.) ;
#5842 = EDGE_CURVE('',#4696,#4697,#4021,.T.) ;
#5843 = EDGE_CURVE('',#4697,#4698,#2714,.T.) ;
#5844 = EDGE_CURVE('',#4699,#4698,#4022,.T.) ;
#5845 = EDGE_CURVE('',#4699,#4700,#2715,.T.) ;
#5846 = EDGE_CURVE('',#4700,#4701,#4023,.T.) ;
#5847 = EDGE_CURVE('',#4701,#4702,#2716,.T.) ;
#5848 = EDGE_CURVE('',#4703,#4702,#4024,.T.) ;
#5849 = EDGE_CURVE('',#4703,#4704,#2717,.T.) ;
#5850 = EDGE_CURVE('',#4704,#4705,#4025,.T.) ;
#5851 = EDGE_CURVE('',#4705,#4706,#2718,.T.) ;
#5852 = EDGE_CURVE('',#4707,#4706,#4026,.T.) ;
#5853 = EDGE_CURVE('',#4707,#4708,#2719,.T.) ;
#5854 = EDGE_CURVE('',#4708,#4709,#4027,.T.) ;
#5855 = EDGE_CURVE('',#4709,#4710,#2720,.T.) ;
#5856 = EDGE_CURVE('',#4711,#4710,#4028,.T.) ;
#5857 = EDGE_CURVE('',#4711,#4712,#2721,.T.) ;
#5858 = EDGE_CURVE('',#4712,#4713,#4029,.T.) ;
#5859 = EDGE_CURVE('',#4713,#4714,#2722,.T.) ;
#5860 = EDGE_CURVE('',#4715,#4714,#4030,.T.) ;
#5861 = EDGE_CURVE('',#4715,#4716,#2723,.T.) ;
#5862 = EDGE_CURVE('',#4716,#4717,#4031,.T.) ;
#5863 = EDGE_CURVE('',#4717,#4718,#2724,.T.) ;
#5864 = EDGE_CURVE('',#4719,#4718,#4032,.T.) ;
#5865 = EDGE_CURVE('',#4719,#4720,#2725,.T.) ;
#5866 = EDGE_CURVE('',#4720,#4721,#4033,.T.) ;
#5867 = EDGE_CURVE('',#4721,#4722,#2726,.T.) ;
#5868 = EDGE_CURVE('',#4723,#4722,#4034,.T.) ;
#5869 = EDGE_CURVE('',#4723,#4724,#2727,.T.) ;
#5870 = EDGE_CURVE('',#4724,#4725,#4035,.T.) ;
#5871 = EDGE_CURVE('',#4725,#4726,#2728,.T.) ;
#5872 = EDGE_CURVE('',#4727,#4726,#4036,.T.) ;
#5873 = EDGE_CURVE('',#4727,#4728,#2729,.T.) ;
#5874 = EDGE_CURVE('',#4728,#4729,#4037,.T.) ;
#5875 = EDGE_CURVE('',#4729,#4730,#2730,.T.) ;
#5876 = EDGE_CURVE('',#4731,#4730,#4038,.T.) ;
#5877 = EDGE_CURVE('',#4731,#4732,#2731,.T.) ;
#5878 = EDGE_CURVE('',#4732,#4733,#4039,.T.) ;
#5879 = EDGE_CURVE('',#4733,#4734,#2732,.T.) ;
#5880 = EDGE_CURVE('',#4735,#4734,#4040,.T.) ;
#5881 = EDGE_CURVE('',#4735,#4736,#2733,.T.) ;
#5882 = EDGE_CURVE('',#4736,#4737,#4041,.T.) ;
#5883 = EDGE_CURVE('',#4737,#4738,#2734,.T.) ;
#5884 = EDGE_CURVE('',#4739,#4738,#4042,.T.) ;
#5885 = EDGE_CURVE('',#4739,#4740,#2735,.T.) ;
#5886 = EDGE_CURVE('',#4740,#4741,#4043,.T.) ;
#5887 = EDGE_CURVE('',#4741,#4742,#2736,.T.) ;
#5888 = EDGE_CURVE('',#4743,#4742,#4044,.T.) ;
#5889 = EDGE_CURVE('',#4743,#4744,#2737,.T.) ;
#5890 = EDGE_CURVE('',#4744,#4745,#4045,.T.) ;
#5891 = EDGE_CURVE('',#4745,#4746,#2738,.T.) ;
#5892 = EDGE_CURVE('',#4747,#4746,#4046,.T.) ;
#5893 = EDGE_CURVE('',#4747,#4748,#2739,.T.) ;
#5894 = EDGE_CURVE('',#4748,#4749,#4047,.T.) ;
#5895 = EDGE_CURVE('',#4749,#4750,#2740,.T.) ;
#5896 = EDGE_CURVE('',#4751,#4750,#4048,.T.) ;
#5897 = EDGE_CURVE('',#4751,#4752,#2741,.T.) ;
#5898 = EDGE_CURVE('',#4752,#4753,#4049,.T.) ;
#5899 = EDGE_CURVE('',#4753,#4754,#2742,.T.) ;
#5900 = EDGE_CURVE('',#4754,#4754,#4050,.T.) ;
#5901 = EDGE_CURVE('',#4753,#4755,#4051,.T.) ;
#5902 = EDGE_CURVE('',#4755,#4756,#2743,.T.) ;
#5903 = EDGE_CURVE('',#4757,#4756,#4052,.T.) ;
#5904 = EDGE_CURVE('',#4757,#4758,#2744,.T.) ;
#5905 = EDGE_CURVE('',#4758,#4759,#4053,.T.) ;
#5906 = EDGE_CURVE('',#4759,#4760,#2745,.T.) ;
#5907 = EDGE_CURVE('',#4761,#4760,#4054,.T.) ;
#5908 = EDGE_CURVE('',#4761,#4762,#2746,.T.) ;
#5909 = EDGE_CURVE('',#4762,#4763,#4055,.T.) ;
#5910 = EDGE_CURVE('',#4763,#4764,#2747,.T.) ;
#5911 = EDGE_CURVE('',#4765,#4764,#4056,.T.) ;
#5912 = EDGE_CURVE('',#4765,#4766,#2748,.T.) ;
#5913 = EDGE_CURVE('',#4766,#4767,#4057,.T.) ;
#5914 = EDGE_CURVE('',#4767,#4768,#2749,.T.) ;
#5915 = EDGE_CURVE('',#4769,#4768,#4058,.T.) ;
#5916 = EDGE_CURVE('',#4769,#4770,#2750,.T.) ;
#5917 = EDGE_CURVE('',#4770,#4771,#4059,.T.) ;
#5918 = EDGE_CURVE('',#4771,#4772,#2751,.T.) ;
#5919 = EDGE_CURVE('',#4773,#4772,#4060,.T.) ;
#5920 = EDGE_CURVE('',#4773,#4774,#2752,.T.) ;
#5921 = EDGE_CURVE('',#4774,#4775,#4061,.T.) ;
#5922 = EDGE_CURVE('',#4775,#4776,#2753,.T.) ;
#5923 = EDGE_CURVE('',#4777,#4776,#4062,.T.) ;
#5924 = EDGE_CURVE('',#4777,#4778,#2754,.T.) ;
#5925 = EDGE_CURVE('',#4778,#4779,#4063,.T.) ;
#5926 = EDGE_CURVE('',#4779,#4780,#2755,.T.) ;
#5927 = EDGE_CURVE('',#4781,#4780,#4064,.T.) ;
#5928 = EDGE_CURVE('',#4781,#4782,#2756,.T.) ;
#5929 = EDGE_CURVE('',#4782,#4783,#4065,.T.) ;
#5930 = EDGE_CURVE('',#4783,#4784,#2757,.T.) ;
#5931 = EDGE_CURVE('',#4785,#4784,#4066,.T.) ;
#5932 = EDGE_CURVE('',#4785,#4786,#2758,.T.) ;
#5933 = EDGE_CURVE('',#4786,#4787,#4067,.T.) ;
#5934 = EDGE_CURVE('',#4787,#4788,#2759,.T.) ;
#5935 = EDGE_CURVE('',#4789,#4788,#4068,.T.) ;
#5936 = EDGE_CURVE('',#4789,#4790,#2760,.T.) ;
#5937 = EDGE_CURVE('',#4790,#4791,#4069,.T.) ;
#5938 = EDGE_CURVE('',#4791,#4792,#2761,.T.) ;
#5939 = EDGE_CURVE('',#4793,#4792,#4070,.T.) ;
#5940 = EDGE_CURVE('',#4793,#4794,#2762,.T.) ;
#5941 = EDGE_CURVE('',#4794,#4795,#4071,.T.) ;
#5942 = EDGE_CURVE('',#4795,#4796,#2763,.T.) ;
#5943 = EDGE_CURVE('',#4797,#4796,#4072,.T.) ;
#5944 = EDGE_CURVE('',#4797,#4798,#2764,.T.) ;
#5945 = EDGE_CURVE('',#4798,#4799,#4073,.T.) ;
#5946 = EDGE_CURVE('',#4799,#4800,#2765,.T.) ;
#5947 = EDGE_CURVE('',#4801,#4800,#4074,.T.) ;
#5948 = EDGE_CURVE('',#4801,#4802,#2766,.T.) ;
#5949 = EDGE_CURVE('',#4802,#4803,#4075,.T.) ;
#5950 = EDGE_CURVE('',#4803,#4804,#2767,.T.) ;
#5951 = EDGE_CURVE('',#4805,#4804,#4076,.T.) ;
#5952 = EDGE_CURVE('',#4805,#4806,#2768,.T.) ;
#5953 = EDGE_CURVE('',#4806,#4807,#4077,.T.) ;
#5954 = EDGE_CURVE('',#4807,#4808,#2769,.T.) ;
#5955 = EDGE_CURVE('',#4809,#4808,#4078,.T.) ;
#5956 = EDGE_CURVE('',#4809,#4810,#2770,.T.) ;
#5957 = EDGE_CURVE('',#4810,#4811,#4079,.T.) ;
#5958 = EDGE_CURVE('',#4811,#4812,#2771,.T.) ;
#5959 = EDGE_CURVE('',#4813,#4812,#4080,.T.) ;
#5960 = EDGE_CURVE('',#4813,#4814,#2772,.T.) ;
#5961 = EDGE_CURVE('',#4814,#4815,#4081,.T.) ;
#5962 = EDGE_CURVE('',#4815,#4816,#2773,.T.) ;
#5963 = EDGE_CURVE('',#4817,#4816,#4082,.T.) ;
#5964 = EDGE_CURVE('',#4817,#4818,#2774,.T.) ;
#5965 = EDGE_CURVE('',#4818,#4819,#4083,.T.) ;
#5966 = EDGE_CURVE('',#4819,#4820,#2775,.T.) ;
#5967 = EDGE_CURVE('',#4678,#4820,#4084,.T.) ;
#5968 = EDGE_CURVE('',#4819,#4821,#2776,.T.) ;
#5969 = EDGE_CURVE('',#4822,#4821,#2777,.T.) ;
#5970 = EDGE_CURVE('',#4820,#4822,#249,.T.) ;
#5971 = EDGE_CURVE('',#4822,#4817,#250,.T.) ;
#5972 = EDGE_CURVE('',#4821,#4818,#2778,.T.) ;
#5973 = EDGE_CURVE('',#4823,#4823,#4085,.T.) ;
#5974 = EDGE_CURVE('',#4823,#4824,#2779,.T.) ;
#5975 = EDGE_CURVE('',#4824,#4751,#251,.T.) ;
#5976 = EDGE_CURVE('',#4750,#4825,#252,.T.) ;
#5977 = EDGE_CURVE('',#4825,#4747,#253,.T.) ;
#5978 = EDGE_CURVE('',#4746,#4826,#254,.T.) ;
#5979 = EDGE_CURVE('',#4826,#4743,#255,.T.) ;
#5980 = EDGE_CURVE('',#4742,#4827,#256,.T.) ;
#5981 = EDGE_CURVE('',#4827,#4739,#257,.T.) ;
#5982 = EDGE_CURVE('',#4738,#4828,#258,.T.) ;
#5983 = EDGE_CURVE('',#4828,#4735,#259,.T.) ;
#5984 = EDGE_CURVE('',#4734,#4829,#260,.T.) ;
#5985 = EDGE_CURVE('',#4829,#4731,#261,.T.) ;
#5986 = EDGE_CURVE('',#4730,#4830,#262,.T.) ;
#5987 = EDGE_CURVE('',#4830,#4727,#263,.T.) ;
#5988 = EDGE_CURVE('',#4726,#4831,#264,.T.) ;
#5989 = EDGE_CURVE('',#4831,#4723,#265,.T.) ;
#5990 = EDGE_CURVE('',#4722,#4832,#266,.T.) ;
#5991 = EDGE_CURVE('',#4832,#4719,#267,.T.) ;
#5992 = EDGE_CURVE('',#4718,#4833,#268,.T.) ;
#5993 = EDGE_CURVE('',#4833,#4715,#269,.T.) ;
#5994 = EDGE_CURVE('',#4714,#4834,#270,.T.) ;
#5995 = EDGE_CURVE('',#4834,#4711,#271,.T.) ;
#5996 = EDGE_CURVE('',#4710,#4835,#272,.T.) ;
#5997 = EDGE_CURVE('',#4835,#4707,#273,.T.) ;
#5998 = EDGE_CURVE('',#4706,#4836,#274,.T.) ;
#5999 = EDGE_CURVE('',#4836,#4703,#275,.T.) ;
#6000 = EDGE_CURVE('',#4702,#4837,#276,.T.) ;
#6001 = EDGE_CURVE('',#4837,#4699,#277,.T.) ;
#6002 = EDGE_CURVE('',#4698,#4838,#278,.T.) ;
#6003 = EDGE_CURVE('',#4838,#4695,#279,.T.) ;
#6004 = EDGE_CURVE('',#4694,#4839,#280,.T.) ;
#6005 = EDGE_CURVE('',#4839,#4691,#281,.T.) ;
#6006 = EDGE_CURVE('',#4690,#4840,#282,.T.) ;
#6007 = EDGE_CURVE('',#4840,#4687,#283,.T.) ;
#6008 = EDGE_CURVE('',#4686,#4841,#284,.T.) ;
#6009 = EDGE_CURVE('',#4841,#4683,#285,.T.) ;
#6010 = EDGE_CURVE('',#4682,#4842,#286,.T.) ;
#6011 = EDGE_CURVE('',#4842,#4679,#287,.T.) ;
#6012 = EDGE_CURVE('',#4816,#4843,#288,.T.) ;
#6013 = EDGE_CURVE('',#4843,#4813,#289,.T.) ;
#6014 = EDGE_CURVE('',#4812,#4844,#290,.T.) ;
#6015 = EDGE_CURVE('',#4844,#4809,#291,.T.) ;
#6016 = EDGE_CURVE('',#4808,#4845,#292,.T.) ;
#6017 = EDGE_CURVE('',#4845,#4805,#293,.T.) ;
#6018 = EDGE_CURVE('',#4804,#4846,#294,.T.) ;
#6019 = EDGE_CURVE('',#4846,#4801,#295,.T.) ;
#6020 = EDGE_CURVE('',#4800,#4847,#296,.T.) ;
#6021 = EDGE_CURVE('',#4847,#4797,#297,.T.) ;
#6022 = EDGE_CURVE('',#4796,#4848,#298,.T.) ;
#6023 = EDGE_CURVE('',#4848,#4793,#299,.T.) ;
#6024 = EDGE_CURVE('',#4792,#4849,#300,.T.) ;
#6025 = EDGE_CURVE('',#4849,#4789,#301,.T.) ;
#6026 = EDGE_CURVE('',#4788,#4850,#302,.T.) ;
#6027 = EDGE_CURVE('',#4850,#4785,#303,.T.) ;
#6028 = EDGE_CURVE('',#4784,#4851,#304,.T.) ;
#6029 = EDGE_CURVE('',#4851,#4781,#305,.T.) ;
#6030 = EDGE_CURVE('',#4780,#4852,#306,.T.) ;
#6031 = EDGE_CURVE('',#4852,#4777,#307,.T.) ;
#6032 = EDGE_CURVE('',#4776,#4853,#308,.T.) ;
#6033 = EDGE_CURVE('',#4853,#4773,#309,.T.) ;
#6034 = EDGE_CURVE('',#4772,#4854,#310,.T.) ;
#6035 = EDGE_CURVE('',#4854,#4769,#311,.T.) ;
#6036 = EDGE_CURVE('',#4768,#4855,#312,.T.) ;
#6037 = EDGE_CURVE('',#4855,#4765,#313,.T.) ;
#6038 = EDGE_CURVE('',#4764,#4856,#314,.T.) ;
#6039 = EDGE_CURVE('',#4856,#4761,#315,.T.) ;
#6040 = EDGE_CURVE('',#4760,#4857,#316,.T.) ;
#6041 = EDGE_CURVE('',#4857,#4757,#317,.T.) ;
#6042 = EDGE_CURVE('',#4756,#4824,#318,.T.) ;
#6043 = EDGE_CURVE('',#4858,#4814,#2780,.T.) ;
#6044 = EDGE_CURVE('',#4815,#4858,#2781,.T.) ;
#6045 = EDGE_CURVE('',#4843,#4858,#2782,.T.) ;
#6046 = EDGE_CURVE('',#4811,#4859,#2783,.T.) ;
#6047 = EDGE_CURVE('',#4844,#4859,#2784,.T.) ;
#6048 = EDGE_CURVE('',#4859,#4810,#2785,.T.) ;
#6049 = EDGE_CURVE('',#4860,#4806,#2786,.T.) ;
#6050 = EDGE_CURVE('',#4807,#4860,#2787,.T.) ;
#6051 = EDGE_CURVE('',#4845,#4860,#2788,.T.) ;
#6052 = EDGE_CURVE('',#4803,#4861,#2789,.T.) ;
#6053 = EDGE_CURVE('',#4846,#4861,#2790,.T.) ;
#6054 = EDGE_CURVE('',#4861,#4802,#2791,.T.) ;
#6055 = EDGE_CURVE('',#4862,#4798,#2792,.T.) ;
#6056 = EDGE_CURVE('',#4799,#4862,#2793,.T.) ;
#6057 = EDGE_CURVE('',#4847,#4862,#2794,.T.) ;
#6058 = EDGE_CURVE('',#4795,#4863,#2795,.T.) ;
#6059 = EDGE_CURVE('',#4848,#4863,#2796,.T.) ;
#6060 = EDGE_CURVE('',#4863,#4794,#2797,.T.) ;
#6061 = EDGE_CURVE('',#4864,#4790,#2798,.T.) ;
#6062 = EDGE_CURVE('',#4791,#4864,#2799,.T.) ;
#6063 = EDGE_CURVE('',#4849,#4864,#2800,.T.) ;
#6064 = EDGE_CURVE('',#4787,#4865,#2801,.T.) ;
#6065 = EDGE_CURVE('',#4850,#4865,#2802,.T.) ;
#6066 = EDGE_CURVE('',#4865,#4786,#2803,.T.) ;
#6067 = EDGE_CURVE('',#4866,#4782,#2804,.T.) ;
#6068 = EDGE_CURVE('',#4783,#4866,#2805,.T.) ;
#6069 = EDGE_CURVE('',#4851,#4866,#2806,.T.) ;
#6070 = EDGE_CURVE('',#4779,#4867,#2807,.T.) ;
#6071 = EDGE_CURVE('',#4852,#4867,#2808,.T.) ;
#6072 = EDGE_CURVE('',#4867,#4778,#2809,.T.) ;
#6073 = EDGE_CURVE('',#4868,#4774,#2810,.T.) ;
#6074 = EDGE_CURVE('',#4775,#4868,#2811,.T.) ;
#6075 = EDGE_CURVE('',#4853,#4868,#2812,.T.) ;
#6076 = EDGE_CURVE('',#4771,#4869,#2813,.T.) ;
#6077 = EDGE_CURVE('',#4854,#4869,#2814,.T.) ;
#6078 = EDGE_CURVE('',#4869,#4770,#2815,.T.) ;
#6079 = EDGE_CURVE('',#4870,#4766,#2816,.T.) ;
#6080 = EDGE_CURVE('',#4767,#4870,#2817,.T.) ;
#6081 = EDGE_CURVE('',#4855,#4870,#2818,.T.) ;
#6082 = EDGE_CURVE('',#4763,#4871,#2819,.T.) ;
#6083 = EDGE_CURVE('',#4856,#4871,#2820,.T.) ;
#6084 = EDGE_CURVE('',#4871,#4762,#2821,.T.) ;
#6085 = EDGE_CURVE('',#4872,#4758,#2822,.T.) ;
#6086 = EDGE_CURVE('',#4759,#4872,#2823,.T.) ;
#6087 = EDGE_CURVE('',#4857,#4872,#2824,.T.) ;
#6088 = EDGE_CURVE('',#4755,#4873,#2825,.T.) ;
#6089 = EDGE_CURVE('',#4824,#4873,#2826,.T.) ;
#6090 = EDGE_CURVE('',#4873,#4752,#2827,.T.) ;
#6091 = EDGE_CURVE('',#4874,#4748,#2828,.T.) ;
#6092 = EDGE_CURVE('',#4749,#4874,#2829,.T.) ;
#6093 = EDGE_CURVE('',#4825,#4874,#2830,.T.) ;
#6094 = EDGE_CURVE('',#4745,#4875,#2831,.T.) ;
#6095 = EDGE_CURVE('',#4826,#4875,#2832,.T.) ;
#6096 = EDGE_CURVE('',#4875,#4744,#2833,.T.) ;
#6097 = EDGE_CURVE('',#4876,#4740,#2834,.T.) ;
#6098 = EDGE_CURVE('',#4741,#4876,#2835,.T.) ;
#6099 = EDGE_CURVE('',#4827,#4876,#2836,.T.) ;
#6100 = EDGE_CURVE('',#4737,#4877,#2837,.T.) ;
#6101 = EDGE_CURVE('',#4828,#4877,#2838,.T.) ;
#6102 = EDGE_CURVE('',#4877,#4736,#2839,.T.) ;
#6103 = EDGE_CURVE('',#4878,#4732,#2840,.T.) ;
#6104 = EDGE_CURVE('',#4733,#4878,#2841,.T.) ;
#6105 = EDGE_CURVE('',#4829,#4878,#2842,.T.) ;
#6106 = EDGE_CURVE('',#4729,#4879,#2843,.T.) ;
#6107 = EDGE_CURVE('',#4830,#4879,#2844,.T.) ;
#6108 = EDGE_CURVE('',#4879,#4728,#2845,.T.) ;
#6109 = EDGE_CURVE('',#4880,#4724,#2846,.T.) ;
#6110 = EDGE_CURVE('',#4725,#4880,#2847,.T.) ;
#6111 = EDGE_CURVE('',#4831,#4880,#2848,.T.) ;
#6112 = EDGE_CURVE('',#4721,#4881,#2849,.T.) ;
#6113 = EDGE_CURVE('',#4832,#4881,#2850,.T.) ;
#6114 = EDGE_CURVE('',#4881,#4720,#2851,.T.) ;
#6115 = EDGE_CURVE('',#4882,#4716,#2852,.T.) ;
#6116 = EDGE_CURVE('',#4717,#4882,#2853,.T.) ;
#6117 = EDGE_CURVE('',#4833,#4882,#2854,.T.) ;
#6118 = EDGE_CURVE('',#4713,#4883,#2855,.T.) ;
#6119 = EDGE_CURVE('',#4834,#4883,#2856,.T.) ;
#6120 = EDGE_CURVE('',#4883,#4712,#2857,.T.) ;
#6121 = EDGE_CURVE('',#4884,#4708,#2858,.T.) ;
#6122 = EDGE_CURVE('',#4709,#4884,#2859,.T.) ;
#6123 = EDGE_CURVE('',#4835,#4884,#2860,.T.) ;
#6124 = EDGE_CURVE('',#4705,#4885,#2861,.T.) ;
#6125 = EDGE_CURVE('',#4836,#4885,#2862,.T.) ;
#6126 = EDGE_CURVE('',#4885,#4704,#2863,.T.) ;
#6127 = EDGE_CURVE('',#4886,#4700,#2864,.T.) ;
#6128 = EDGE_CURVE('',#4701,#4886,#2865,.T.) ;
#6129 = EDGE_CURVE('',#4837,#4886,#2866,.T.) ;
#6130 = EDGE_CURVE('',#4697,#4887,#2867,.T.) ;
#6131 = EDGE_CURVE('',#4838,#4887,#2868,.T.) ;
#6132 = EDGE_CURVE('',#4887,#4696,#2869,.T.) ;
#6133 = EDGE_CURVE('',#4888,#4692,#2870,.T.) ;
#6134 = EDGE_CURVE('',#4693,#4888,#2871,.T.) ;
#6135 = EDGE_CURVE('',#4839,#4888,#2872,.T.) ;
#6136 = EDGE_CURVE('',#4689,#4889,#2873,.T.) ;
#6137 = EDGE_CURVE('',#4840,#4889,#2874,.T.) ;
#6138 = EDGE_CURVE('',#4889,#4688,#2875,.T.) ;
#6139 = EDGE_CURVE('',#4890,#4684,#2876,.T.) ;
#6140 = EDGE_CURVE('',#4685,#4890,#2877,.T.) ;
#6141 = EDGE_CURVE('',#4841,#4890,#2878,.T.) ;
#6142 = EDGE_CURVE('',#4681,#4891,#2879,.T.) ;
#6143 = EDGE_CURVE('',#4842,#4891,#2880,.T.) ;
#6144 = EDGE_CURVE('',#4891,#4680,#2881,.T.) ;
#6145 = EDGE_CURVE('',#4671,#4754,#4086,.T.) ;
#6146 = EDGE_CURVE('',#4892,#4892,#4087,.T.) ;
#6147 = EDGE_CURVE('',#4892,#4893,#2882,.T.) ;
#6148 = EDGE_CURVE('',#4894,#4893,#319,.T.) ;
#6149 = EDGE_CURVE('',#4894,#4895,#4088,.T.) ;
#6150 = EDGE_CURVE('',#4896,#4895,#320,.T.) ;
#6151 = EDGE_CURVE('',#4897,#4896,#321,.T.) ;
#6152 = EDGE_CURVE('',#4897,#4898,#4089,.T.) ;
#6153 = EDGE_CURVE('',#4899,#4898,#322,.T.) ;
#6154 = EDGE_CURVE('',#4900,#4899,#323,.T.) ;
#6155 = EDGE_CURVE('',#4900,#4901,#4090,.T.) ;
#6156 = EDGE_CURVE('',#4902,#4901,#324,.T.) ;
#6157 = EDGE_CURVE('',#4903,#4902,#325,.T.) ;
#6158 = EDGE_CURVE('',#4903,#4904,#4091,.T.) ;
#6159 = EDGE_CURVE('',#4905,#4904,#326,.T.) ;
#6160 = EDGE_CURVE('',#4906,#4905,#327,.T.) ;
#6161 = EDGE_CURVE('',#4906,#4907,#4092,.T.) ;
#6162 = EDGE_CURVE('',#4908,#4907,#328,.T.) ;
#6163 = EDGE_CURVE('',#4909,#4908,#329,.T.) ;
#6164 = EDGE_CURVE('',#4909,#4910,#4093,.T.) ;
#6165 = EDGE_CURVE('',#4893,#4910,#330,.T.) ;
#6166 = EDGE_CURVE('',#4901,#4911,#2883,.T.) ;
#6167 = EDGE_CURVE('',#4912,#4900,#2884,.T.) ;
#6168 = EDGE_CURVE('',#4911,#4912,#4094,.T.) ;
#6169 = EDGE_CURVE('',#4904,#4913,#2885,.T.) ;
#6170 = EDGE_CURVE('',#4914,#4903,#2886,.T.) ;
#6171 = EDGE_CURVE('',#4913,#4914,#4095,.T.) ;
#6172 = EDGE_CURVE('',#4915,#4897,#2887,.T.) ;
#6173 = EDGE_CURVE('',#4916,#4915,#4096,.T.) ;
#6174 = EDGE_CURVE('',#4898,#4916,#2888,.T.) ;
#6175 = EDGE_CURVE('',#4907,#4917,#2889,.T.) ;
#6176 = EDGE_CURVE('',#4918,#4906,#2890,.T.) ;
#6177 = EDGE_CURVE('',#4917,#4918,#4097,.T.) ;
#6178 = EDGE_CURVE('',#4919,#4894,#2891,.T.) ;
#6179 = EDGE_CURVE('',#4920,#4919,#4098,.T.) ;
#6180 = EDGE_CURVE('',#4895,#4920,#2892,.T.) ;
#6181 = EDGE_CURVE('',#4921,#4909,#2893,.T.) ;
#6182 = EDGE_CURVE('',#4922,#4921,#4099,.T.) ;
#6183 = EDGE_CURVE('',#4910,#4922,#2894,.T.) ;
#6184 = EDGE_CURVE('',#4918,#4917,#2895,.T.) ;
#6185 = EDGE_CURVE('',#4905,#4923,#2896,.T.) ;
#6186 = EDGE_CURVE('',#4923,#4924,#2897,.T.) ;
#6187 = EDGE_CURVE('',#4908,#4924,#2898,.T.) ;
#6188 = EDGE_CURVE('',#4914,#4913,#2899,.T.) ;
#6189 = EDGE_CURVE('',#4902,#4925,#2900,.T.) ;
#6190 = EDGE_CURVE('',#4925,#4923,#2901,.T.) ;
#6191 = EDGE_CURVE('',#4912,#4911,#2902,.T.) ;
#6192 = EDGE_CURVE('',#4899,#4926,#2903,.T.) ;
#6193 = EDGE_CURVE('',#4926,#4925,#2904,.T.) ;
#6194 = EDGE_CURVE('',#4915,#4916,#2905,.T.) ;
#6195 = EDGE_CURVE('',#4919,#4920,#2906,.T.) ;
#6196 = EDGE_CURVE('',#4921,#4922,#2907,.T.) ;
#6197 = EDGE_CURVE('',#4927,#4926,#2908,.T.) ;
#6198 = EDGE_CURVE('',#4927,#4926,#4100,.T.) ;
#6199 = EDGE_CURVE('',#4926,#4925,#4101,.T.) ;
#6200 = EDGE_CURVE('',#4925,#4923,#4102,.T.) ;
#6201 = EDGE_CURVE('',#4923,#4924,#4103,.T.) ;
#6202 = EDGE_CURVE('',#4924,#4928,#2909,.T.) ;
#6203 = EDGE_CURVE('',#4924,#4928,#4104,.T.) ;
#6204 = EDGE_CURVE('',#4928,#4927,#2910,.T.) ;
#6205 = EDGE_CURVE('',#4928,#4927,#4105,.T.) ;
#6206 = EDGE_CURVE('',#4928,#4929,#2911,.T.) ;
#6207 = EDGE_CURVE('',#4896,#4927,#2912,.T.) ;
#6208 = EDGE_CURVE('',#4893,#4928,#2913,.T.) ;
#6209 = EDGE_CURVE('',#4930,#4930,#4106,.T.) ;
#6210 = EDGE_CURVE('',#4930,#4931,#2914,.T.) ;
#6211 = EDGE_CURVE('',#4931,#4931,#4107,.T.) ;
#6212 = EDGE_CURVE('',#4932,#4932,#4108,.T.) ;
#6213 = EDGE_CURVE('',#4932,#4933,#2915,.T.) ;
#6214 = EDGE_CURVE('',#4933,#4933,#4109,.T.) ;
#6215 = EDGE_CURVE('',#4934,#4935,#4110,.T.) ;
#6216 = EDGE_CURVE('',#4936,#4934,#2916,.T.) ;
#6217 = EDGE_CURVE('',#4937,#4936,#2917,.T.) ;
#6218 = EDGE_CURVE('',#4937,#4938,#2918,.T.) ;
#6219 = EDGE_CURVE('',#4938,#4939,#2919,.T.) ;
#6220 = EDGE_CURVE('',#4935,#4939,#2920,.T.) ;
#6221 = EDGE_CURVE('',#4940,#4940,#4111,.T.) ;
#6222 = EDGE_CURVE('',#4940,#4941,#2921,.T.) ;
#6223 = EDGE_CURVE('',#4941,#4941,#4112,.T.) ;
#6224 = EDGE_CURVE('',#4942,#4937,#2922,.T.) ;
#6225 = EDGE_CURVE('',#4943,#4936,#2923,.T.) ;
#6226 = EDGE_CURVE('',#4942,#4943,#2924,.T.) ;
#6227 = EDGE_CURVE('',#4944,#4942,#4113,.T.) ;
#6228 = EDGE_CURVE('',#4945,#4943,#4114,.T.) ;
#6229 = EDGE_CURVE('',#4944,#4945,#2925,.T.) ;
#6230 = EDGE_CURVE('',#4938,#4944,#2926,.T.) ;
#6231 = EDGE_CURVE('',#4939,#4945,#2927,.T.) ;
#6232 = EDGE_CURVE('',#4935,#4946,#2928,.T.) ;
#6233 = EDGE_CURVE('',#4947,#4934,#2929,.T.) ;
#6234 = EDGE_CURVE('',#4946,#4947,#2930,.T.) ;
#6235 = EDGE_CURVE('',#4948,#4947,#4115,.T.) ;
#6236 = EDGE_CURVE('',#4949,#4948,#4116,.T.) ;
#6237 = EDGE_CURVE('',#4949,#4950,#2931,.T.) ;
#6238 = EDGE_CURVE('',#4946,#4950,#4117,.T.) ;
#6239 = EDGE_CURVE('',#4950,#4951,#2932,.T.) ;
#6240 = EDGE_CURVE('',#4952,#4949,#2933,.T.) ;
#6241 = EDGE_CURVE('',#4953,#4952,#2934,.T.) ;
#6242 = EDGE_CURVE('',#4954,#4953,#2935,.T.) ;
#6243 = EDGE_CURVE('',#4955,#4954,#4118,.T.) ;
#6244 = EDGE_CURVE('',#4956,#4955,#2936,.T.) ;
#6245 = EDGE_CURVE('',#4951,#4956,#2937,.T.) ;
#6246 = EDGE_CURVE('',#4957,#4957,#4119,.T.) ;
#6247 = EDGE_CURVE('',#4958,#4958,#4120,.T.) ;
#6248 = EDGE_CURVE('',#4958,#4957,#2938,.T.) ;
#6249 = EDGE_CURVE('',#4953,#4959,#2939,.T.) ;
#6250 = EDGE_CURVE('',#4960,#4959,#2940,.T.) ;
#6251 = EDGE_CURVE('',#4954,#4960,#2941,.T.) ;
#6252 = EDGE_CURVE('',#4961,#4960,#4121,.T.) ;
#6253 = EDGE_CURVE('',#4955,#4961,#2942,.T.) ;
#6254 = EDGE_CURVE('',#4962,#4961,#2943,.T.) ;
#6255 = EDGE_CURVE('',#4956,#4962,#2944,.T.) ;
#6256 = EDGE_CURVE('',#4951,#4952,#4122,.T.) ;
#6257 = EDGE_CURVE('',#4959,#4962,#2945,.T.) ;
#6258 = EDGE_CURVE('',#4963,#4963,#4123,.T.) ;
#6259 = EDGE_CURVE('',#4963,#4948,#2946,.T.) ;
#6260 = EDGE_CURVE('',#4964,#4964,#4124,.T.) ;
#6261 = EDGE_CURVE('',#4964,#4965,#2947,.T.) ;
#6262 = EDGE_CURVE('',#4965,#4965,#4125,.T.) ;
#6263 = EDGE_CURVE('',#4966,#4967,#2948,.T.) ;
#6264 = EDGE_CURVE('',#4967,#4968,#2949,.T.) ;
#6265 = EDGE_CURVE('',#4969,#4968,#2950,.T.) ;
#6266 = EDGE_CURVE('',#4966,#4969,#2951,.T.) ;
#6267 = EDGE_CURVE('',#4970,#4966,#2952,.T.) ;
#6268 = EDGE_CURVE('',#4971,#4969,#2953,.T.) ;
#6269 = EDGE_CURVE('',#4970,#4971,#2954,.T.) ;
#6270 = EDGE_CURVE('',#4972,#4970,#2955,.T.) ;
#6271 = EDGE_CURVE('',#4973,#4971,#2956,.T.) ;
#6272 = EDGE_CURVE('',#4972,#4973,#2957,.T.) ;
#6273 = EDGE_CURVE('',#4967,#4972,#2958,.T.) ;
#6274 = EDGE_CURVE('',#4968,#4973,#2959,.T.) ;
#6275 = EDGE_CURVE('',#4974,#4974,#4126,.T.) ;
#6276 = EDGE_CURVE('',#4974,#4975,#2960,.T.) ;
#6277 = EDGE_CURVE('',#4975,#4975,#4127,.T.) ;
#6278 = EDGE_CURVE('',#4976,#4976,#4128,.T.) ;
#6279 = EDGE_CURVE('',#4976,#4977,#2961,.T.) ;
#6280 = EDGE_CURVE('',#4977,#4977,#4129,.T.) ;
#6281 = EDGE_CURVE('',#4978,#4979,#2962,.T.) ;
#6282 = EDGE_CURVE('',#4978,#4980,#2963,.T.) ;
#6283 = EDGE_CURVE('',#4980,#4981,#4130,.T.) ;
#6284 = EDGE_CURVE('',#4981,#4979,#2964,.T.) ;
#6285 = EDGE_CURVE('',#4982,#4982,#4131,.T.) ;
#6286 = EDGE_CURVE('',#4983,#4978,#2965,.T.) ;
#6287 = EDGE_CURVE('',#4983,#4984,#2966,.T.) ;
#6288 = EDGE_CURVE('',#4984,#4980,#2967,.T.) ;
#6289 = EDGE_CURVE('',#4982,#4985,#2968,.T.) ;
#6290 = EDGE_CURVE('',#4985,#4985,#4132,.T.) ;
#6291 = EDGE_CURVE('',#4979,#4986,#2969,.T.) ;
#6292 = EDGE_CURVE('',#4987,#4981,#2970,.T.) ;
#6293 = EDGE_CURVE('',#4987,#4986,#2971,.T.) ;
#6294 = EDGE_CURVE('',#4984,#4987,#4133,.T.) ;
#6295 = EDGE_CURVE('',#4986,#4983,#2972,.T.) ;
#6296 = EDGE_CURVE('',#4988,#4989,#2973,.T.) ;
#6297 = EDGE_CURVE('',#4988,#4990,#2974,.T.) ;
#6298 = EDGE_CURVE('',#4990,#4991,#4134,.T.) ;
#6299 = EDGE_CURVE('',#4991,#4989,#2975,.T.) ;
#6300 = EDGE_CURVE('',#4992,#4992,#4135,.T.) ;
#6301 = EDGE_CURVE('',#4993,#4988,#2976,.T.) ;
#6302 = EDGE_CURVE('',#4993,#4994,#2977,.T.) ;
#6303 = EDGE_CURVE('',#4994,#4990,#2978,.T.) ;
#6304 = EDGE_CURVE('',#4992,#4995,#2979,.T.) ;
#6305 = EDGE_CURVE('',#4995,#4995,#4136,.T.) ;
#6306 = EDGE_CURVE('',#4989,#4996,#2980,.T.) ;
#6307 = EDGE_CURVE('',#4997,#4991,#2981,.T.) ;
#6308 = EDGE_CURVE('',#4997,#4996,#2982,.T.) ;
#6309 = EDGE_CURVE('',#4994,#4997,#4137,.T.) ;
#6310 = EDGE_CURVE('',#4996,#4993,#2983,.T.) ;
#6311 = EDGE_CURVE('',#4998,#4999,#2984,.T.) ;
#6312 = EDGE_CURVE('',#4999,#5000,#2985,.T.) ;
#6313 = EDGE_CURVE('',#5001,#5000,#2986,.T.) ;
#6314 = EDGE_CURVE('',#4998,#5001,#2987,.T.) ;
#6315 = EDGE_CURVE('',#5002,#4998,#2988,.T.) ;
#6316 = EDGE_CURVE('',#5003,#5001,#2989,.T.) ;
#6317 = EDGE_CURVE('',#5002,#5003,#2990,.T.) ;
#6318 = EDGE_CURVE('',#5004,#5002,#2991,.T.) ;
#6319 = EDGE_CURVE('',#5005,#5003,#2992,.T.) ;
#6320 = EDGE_CURVE('',#5004,#5005,#2993,.T.) ;
#6321 = EDGE_CURVE('',#4999,#5004,#2994,.T.) ;
#6322 = EDGE_CURVE('',#5000,#5005,#2995,.T.) ;
#6323 = EDGE_CURVE('',#5006,#5006,#4138,.T.) ;
#6324 = EDGE_CURVE('',#5007,#5007,#4139,.T.) ;
#6325 = EDGE_CURVE('',#5008,#5008,#4140,.T.) ;
#6326 = EDGE_CURVE('',#5008,#5006,#2996,.T.) ;
#6327 = EDGE_CURVE('',#5009,#5009,#4141,.T.) ;
#6328 = EDGE_CURVE('',#5010,#5010,#4142,.T.) ;
#6329 = EDGE_CURVE('',#5010,#5009,#2997,.T.) ;
#6330 = EDGE_CURVE('',#5011,#5011,#4143,.T.) ;
#6331 = EDGE_CURVE('',#5011,#5010,#2998,.T.) ;
#6332 = EDGE_CURVE('',#5012,#5012,#4144,.T.) ;
#6333 = EDGE_CURVE('',#5012,#5011,#2999,.T.) ;
#6334 = EDGE_CURVE('',#5013,#5013,#4145,.T.) ;
#6335 = EDGE_CURVE('',#5013,#5012,#3000,.T.) ;
#6336 = EDGE_CURVE('',#5014,#5014,#4146,.T.) ;
#6337 = EDGE_CURVE('',#5014,#5013,#3001,.T.) ;
#6338 = EDGE_CURVE('',#5015,#5015,#4147,.T.) ;
#6339 = EDGE_CURVE('',#5016,#5016,#4148,.T.) ;
#6340 = EDGE_CURVE('',#5016,#5015,#3002,.T.) ;
#6341 = EDGE_CURVE('',#5017,#5017,#4149,.T.) ;
#6342 = EDGE_CURVE('',#5017,#5007,#3003,.T.) ;
#6343 = ORIENTED_EDGE('',*,*,#5018,.T.) ;
#6344 = ORIENTED_EDGE('',*,*,#5019,.T.) ;
#6345 = ORIENTED_EDGE('',*,*,#5020,.T.) ;
#6346 = ORIENTED_EDGE('',*,*,#5019,.F.) ;
#6347 = ORIENTED_EDGE('',*,*,#5021,.F.) ;
#6348 = ORIENTED_EDGE('',*,*,#5022,.F.) ;
#6349 = ORIENTED_EDGE('',*,*,#5023,.F.) ;
#6350 = ORIENTED_EDGE('',*,*,#5024,.F.) ;
#6351 = ORIENTED_EDGE('',*,*,#5025,.F.) ;
#6352 = ORIENTED_EDGE('',*,*,#5018,.F.) ;
#6353 = ORIENTED_EDGE('',*,*,#5020,.F.) ;
#6354 = ORIENTED_EDGE('',*,*,#5026,.T.) ;
#6355 = ORIENTED_EDGE('',*,*,#5027,.T.) ;
#6356 = ORIENTED_EDGE('',*,*,#5026,.F.) ;
#6357 = ORIENTED_EDGE('',*,*,#5028,.T.) ;
#6358 = ORIENTED_EDGE('',*,*,#5029,.T.) ;
#6359 = ORIENTED_EDGE('',*,*,#5030,.T.) ;
#6360 = ORIENTED_EDGE('',*,*,#5029,.F.) ;
#6361 = ORIENTED_EDGE('',*,*,#5031,.F.) ;
#6362 = ORIENTED_EDGE('',*,*,#5032,.F.) ;
#6363 = ORIENTED_EDGE('',*,*,#5033,.F.) ;
#6364 = ORIENTED_EDGE('',*,*,#5034,.F.) ;
#6365 = ORIENTED_EDGE('',*,*,#5035,.F.) ;
#6366 = ORIENTED_EDGE('',*,*,#5028,.F.) ;
#6367 = ORIENTED_EDGE('',*,*,#5030,.F.) ;
#6368 = ORIENTED_EDGE('',*,*,#5036,.T.) ;
#6369 = ORIENTED_EDGE('',*,*,#5037,.T.) ;
#6370 = ORIENTED_EDGE('',*,*,#5036,.F.) ;
#6371 = ORIENTED_EDGE('',*,*,#5038,.T.) ;
#6372 = ORIENTED_EDGE('',*,*,#5039,.T.) ;
#6373 = ORIENTED_EDGE('',*,*,#5040,.T.) ;
#6374 = ORIENTED_EDGE('',*,*,#5039,.F.) ;
#6375 = ORIENTED_EDGE('',*,*,#5041,.F.) ;
#6376 = ORIENTED_EDGE('',*,*,#5042,.F.) ;
#6377 = ORIENTED_EDGE('',*,*,#5043,.F.) ;
#6378 = ORIENTED_EDGE('',*,*,#5044,.F.) ;
#6379 = ORIENTED_EDGE('',*,*,#5045,.F.) ;
#6380 = ORIENTED_EDGE('',*,*,#5038,.F.) ;
#6381 = ORIENTED_EDGE('',*,*,#5040,.F.) ;
#6382 = ORIENTED_EDGE('',*,*,#5046,.T.) ;
#6383 = ORIENTED_EDGE('',*,*,#5047,.T.) ;
#6384 = ORIENTED_EDGE('',*,*,#5046,.F.) ;
#6385 = ORIENTED_EDGE('',*,*,#5048,.T.) ;
#6386 = ORIENTED_EDGE('',*,*,#5049,.T.) ;
#6387 = ORIENTED_EDGE('',*,*,#5050,.T.) ;
#6388 = ORIENTED_EDGE('',*,*,#5049,.F.) ;
#6389 = ORIENTED_EDGE('',*,*,#5051,.F.) ;
#6390 = ORIENTED_EDGE('',*,*,#5052,.F.) ;
#6391 = ORIENTED_EDGE('',*,*,#5053,.F.) ;
#6392 = ORIENTED_EDGE('',*,*,#5054,.F.) ;
#6393 = ORIENTED_EDGE('',*,*,#5055,.F.) ;
#6394 = ORIENTED_EDGE('',*,*,#5048,.F.) ;
#6395 = ORIENTED_EDGE('',*,*,#5050,.F.) ;
#6396 = ORIENTED_EDGE('',*,*,#5056,.T.) ;
#6397 = ORIENTED_EDGE('',*,*,#5057,.T.) ;
#6398 = ORIENTED_EDGE('',*,*,#5056,.F.) ;
#6399 = ORIENTED_EDGE('',*,*,#5045,.T.) ;
#6400 = ORIENTED_EDGE('',*,*,#5058,.T.) ;
#6401 = ORIENTED_EDGE('',*,*,#5059,.T.) ;
#6402 = ORIENTED_EDGE('',*,*,#5058,.F.) ;
#6403 = ORIENTED_EDGE('',*,*,#5059,.F.) ;
#6404 = ORIENTED_EDGE('',*,*,#5060,.T.) ;
#6405 = ORIENTED_EDGE('',*,*,#5061,.T.) ;
#6406 = ORIENTED_EDGE('',*,*,#5062,.F.) ;
#6407 = ORIENTED_EDGE('',*,*,#5063,.T.) ;
#6408 = ORIENTED_EDGE('',*,*,#5060,.F.) ;
#6409 = ORIENTED_EDGE('',*,*,#5055,.T.) ;
#6410 = ORIENTED_EDGE('',*,*,#5064,.T.) ;
#6411 = ORIENTED_EDGE('',*,*,#5065,.T.) ;
#6412 = ORIENTED_EDGE('',*,*,#5064,.F.) ;
#6413 = ORIENTED_EDGE('',*,*,#5065,.F.) ;
#6414 = ORIENTED_EDGE('',*,*,#5066,.T.) ;
#6415 = ORIENTED_EDGE('',*,*,#5067,.T.) ;
#6416 = ORIENTED_EDGE('',*,*,#5068,.F.) ;
#6417 = ORIENTED_EDGE('',*,*,#5069,.T.) ;
#6418 = ORIENTED_EDGE('',*,*,#5066,.F.) ;
#6419 = ORIENTED_EDGE('',*,*,#5035,.T.) ;
#6420 = ORIENTED_EDGE('',*,*,#5070,.T.) ;
#6421 = ORIENTED_EDGE('',*,*,#5071,.T.) ;
#6422 = ORIENTED_EDGE('',*,*,#5070,.F.) ;
#6423 = ORIENTED_EDGE('',*,*,#5071,.F.) ;
#6424 = ORIENTED_EDGE('',*,*,#5072,.T.) ;
#6425 = ORIENTED_EDGE('',*,*,#5073,.T.) ;
#6426 = ORIENTED_EDGE('',*,*,#5072,.F.) ;
#6427 = ORIENTED_EDGE('',*,*,#5025,.T.) ;
#6428 = ORIENTED_EDGE('',*,*,#5074,.T.) ;
#6429 = ORIENTED_EDGE('',*,*,#5075,.T.) ;
#6430 = ORIENTED_EDGE('',*,*,#5074,.F.) ;
#6431 = ORIENTED_EDGE('',*,*,#5075,.F.) ;
#6432 = ORIENTED_EDGE('',*,*,#5076,.T.) ;
#6433 = ORIENTED_EDGE('',*,*,#5077,.T.) ;
#6434 = ORIENTED_EDGE('',*,*,#5076,.F.) ;
#6435 = ORIENTED_EDGE('',*,*,#5027,.F.) ;
#6436 = ORIENTED_EDGE('',*,*,#5078,.T.) ;
#6437 = ORIENTED_EDGE('',*,*,#5078,.F.) ;
#6438 = ORIENTED_EDGE('',*,*,#5077,.F.) ;
#6439 = ORIENTED_EDGE('',*,*,#5079,.T.) ;
#6440 = ORIENTED_EDGE('',*,*,#5079,.F.) ;
#6441 = ORIENTED_EDGE('',*,*,#5037,.F.) ;
#6442 = ORIENTED_EDGE('',*,*,#5080,.T.) ;
#6443 = ORIENTED_EDGE('',*,*,#5080,.F.) ;
#6444 = ORIENTED_EDGE('',*,*,#5073,.F.) ;
#6445 = ORIENTED_EDGE('',*,*,#5081,.T.) ;
#6446 = ORIENTED_EDGE('',*,*,#5081,.F.) ;
#6447 = ORIENTED_EDGE('',*,*,#5082,.F.) ;
#6448 = ORIENTED_EDGE('',*,*,#5067,.F.) ;
#6449 = ORIENTED_EDGE('',*,*,#5069,.F.) ;
#6450 = ORIENTED_EDGE('',*,*,#5083,.F.) ;
#6451 = ORIENTED_EDGE('',*,*,#5084,.T.) ;
#6452 = ORIENTED_EDGE('',*,*,#5085,.F.) ;
#6453 = ORIENTED_EDGE('',*,*,#5084,.F.) ;
#6454 = ORIENTED_EDGE('',*,*,#5082,.T.) ;
#6455 = ORIENTED_EDGE('',*,*,#5068,.T.) ;
#6456 = ORIENTED_EDGE('',*,*,#5057,.F.) ;
#6457 = ORIENTED_EDGE('',*,*,#5086,.T.) ;
#6458 = ORIENTED_EDGE('',*,*,#5086,.F.) ;
#6459 = ORIENTED_EDGE('',*,*,#5087,.F.) ;
#6460 = ORIENTED_EDGE('',*,*,#5061,.F.) ;
#6461 = ORIENTED_EDGE('',*,*,#5063,.F.) ;
#6462 = ORIENTED_EDGE('',*,*,#5088,.F.) ;
#6463 = ORIENTED_EDGE('',*,*,#5089,.T.) ;
#6464 = ORIENTED_EDGE('',*,*,#5090,.F.) ;
#6465 = ORIENTED_EDGE('',*,*,#5089,.F.) ;
#6466 = ORIENTED_EDGE('',*,*,#5087,.T.) ;
#6467 = ORIENTED_EDGE('',*,*,#5062,.T.) ;
#6468 = ORIENTED_EDGE('',*,*,#5047,.F.) ;
#6469 = ORIENTED_EDGE('',*,*,#5091,.T.) ;
#6470 = ORIENTED_EDGE('',*,*,#5091,.F.) ;
#6471 = ORIENTED_EDGE('',*,*,#5092,.F.) ;
#6472 = ORIENTED_EDGE('',*,*,#5093,.F.) ;
#6473 = ORIENTED_EDGE('',*,*,#5094,.T.) ;
#6474 = ORIENTED_EDGE('',*,*,#5095,.F.) ;
#6475 = ORIENTED_EDGE('',*,*,#5096,.F.) ;
#6476 = ORIENTED_EDGE('',*,*,#5094,.F.) ;
#6477 = ORIENTED_EDGE('',*,*,#5097,.F.) ;
#6478 = ORIENTED_EDGE('',*,*,#5098,.T.) ;
#6479 = ORIENTED_EDGE('',*,*,#5099,.T.) ;
#6480 = ORIENTED_EDGE('',*,*,#5098,.F.) ;
#6481 = ORIENTED_EDGE('',*,*,#5095,.T.) ;
#6482 = ORIENTED_EDGE('',*,*,#5096,.T.) ;
#6483 = ORIENTED_EDGE('',*,*,#5099,.F.) ;
#6484 = ORIENTED_EDGE('',*,*,#5100,.F.) ;
#6485 = ORIENTED_EDGE('',*,*,#5101,.F.) ;
#6486 = ORIENTED_EDGE('',*,*,#5102,.T.) ;
#6487 = ORIENTED_EDGE('',*,*,#5103,.F.) ;
#6488 = ORIENTED_EDGE('',*,*,#5104,.F.) ;
#6489 = ORIENTED_EDGE('',*,*,#5102,.F.) ;
#6490 = ORIENTED_EDGE('',*,*,#5105,.F.) ;
#6491 = ORIENTED_EDGE('',*,*,#5106,.T.) ;
#6492 = ORIENTED_EDGE('',*,*,#5107,.T.) ;
#6493 = ORIENTED_EDGE('',*,*,#5106,.F.) ;
#6494 = ORIENTED_EDGE('',*,*,#5103,.T.) ;
#6495 = ORIENTED_EDGE('',*,*,#5104,.T.) ;
#6496 = ORIENTED_EDGE('',*,*,#5107,.F.) ;
#6497 = ORIENTED_EDGE('',*,*,#5108,.F.) ;
#6498 = ORIENTED_EDGE('',*,*,#5109,.T.) ;
#6499 = ORIENTED_EDGE('',*,*,#5110,.F.) ;
#6500 = ORIENTED_EDGE('',*,*,#5109,.F.) ;
#6501 = ORIENTED_EDGE('',*,*,#5111,.F.) ;
#6502 = ORIENTED_EDGE('',*,*,#5112,.T.) ;
#6503 = ORIENTED_EDGE('',*,*,#5113,.F.) ;
#6504 = ORIENTED_EDGE('',*,*,#5112,.F.) ;
#6505 = ORIENTED_EDGE('',*,*,#5114,.F.) ;
#6506 = ORIENTED_EDGE('',*,*,#5115,.F.) ;
#6507 = ORIENTED_EDGE('',*,*,#5116,.F.) ;
#6508 = ORIENTED_EDGE('',*,*,#5117,.F.) ;
#6509 = ORIENTED_EDGE('',*,*,#5118,.F.) ;
#6510 = ORIENTED_EDGE('',*,*,#5119,.F.) ;
#6511 = ORIENTED_EDGE('',*,*,#5120,.F.) ;
#6512 = ORIENTED_EDGE('',*,*,#5121,.F.) ;
#6513 = ORIENTED_EDGE('',*,*,#5120,.T.) ;
#6514 = ORIENTED_EDGE('',*,*,#5122,.F.) ;
#6515 = ORIENTED_EDGE('',*,*,#5123,.F.) ;
#6516 = ORIENTED_EDGE('',*,*,#5124,.T.) ;
#6517 = ORIENTED_EDGE('',*,*,#5119,.T.) ;
#6518 = ORIENTED_EDGE('',*,*,#5125,.T.) ;
#6519 = ORIENTED_EDGE('',*,*,#5126,.T.) ;
#6520 = ORIENTED_EDGE('',*,*,#5127,.F.) ;
#6521 = ORIENTED_EDGE('',*,*,#5128,.T.) ;
#6522 = ORIENTED_EDGE('',*,*,#5122,.T.) ;
#6523 = ORIENTED_EDGE('',*,*,#5113,.T.) ;
#6524 = ORIENTED_EDGE('',*,*,#5116,.T.) ;
#6525 = ORIENTED_EDGE('',*,*,#5129,.F.) ;
#6526 = ORIENTED_EDGE('',*,*,#5130,.F.) ;
#6527 = ORIENTED_EDGE('',*,*,#5131,.T.) ;
#6528 = ORIENTED_EDGE('',*,*,#5115,.T.) ;
#6529 = ORIENTED_EDGE('',*,*,#5132,.T.) ;
#6530 = ORIENTED_EDGE('',*,*,#5133,.T.) ;
#6531 = ORIENTED_EDGE('',*,*,#5134,.F.) ;
#6532 = ORIENTED_EDGE('',*,*,#5135,.T.) ;
#6533 = ORIENTED_EDGE('',*,*,#5129,.T.) ;
#6534 = ORIENTED_EDGE('',*,*,#5110,.T.) ;
#6535 = ORIENTED_EDGE('',*,*,#5136,.T.) ;
#6536 = ORIENTED_EDGE('',*,*,#5137,.T.) ;
#6537 = ORIENTED_EDGE('',*,*,#5138,.T.) ;
#6538 = ORIENTED_EDGE('',*,*,#5139,.T.) ;
#6539 = ORIENTED_EDGE('',*,*,#5139,.F.) ;
#6540 = ORIENTED_EDGE('',*,*,#5140,.F.) ;
#6541 = ORIENTED_EDGE('',*,*,#5141,.T.) ;
#6542 = ORIENTED_EDGE('',*,*,#5142,.T.) ;
#6543 = ORIENTED_EDGE('',*,*,#5143,.T.) ;
#6544 = ORIENTED_EDGE('',*,*,#5144,.T.) ;
#6545 = ORIENTED_EDGE('',*,*,#5090,.T.) ;
#6546 = ORIENTED_EDGE('',*,*,#5138,.F.) ;
#6547 = ORIENTED_EDGE('',*,*,#5145,.F.) ;
#6548 = ORIENTED_EDGE('',*,*,#5146,.T.) ;
#6549 = ORIENTED_EDGE('',*,*,#5147,.T.) ;
#6550 = ORIENTED_EDGE('',*,*,#5148,.T.) ;
#6551 = ORIENTED_EDGE('',*,*,#5149,.F.) ;
#6552 = ORIENTED_EDGE('',*,*,#5150,.T.) ;
#6553 = ORIENTED_EDGE('',*,*,#5151,.T.) ;
#6554 = ORIENTED_EDGE('',*,*,#5152,.T.) ;
#6555 = ORIENTED_EDGE('',*,*,#5153,.F.) ;
#6556 = ORIENTED_EDGE('',*,*,#5154,.F.) ;
#6557 = ORIENTED_EDGE('',*,*,#5155,.F.) ;
#6558 = ORIENTED_EDGE('',*,*,#5156,.F.) ;
#6559 = ORIENTED_EDGE('',*,*,#5157,.F.) ;
#6560 = ORIENTED_EDGE('',*,*,#5053,.T.) ;
#6561 = ORIENTED_EDGE('',*,*,#5158,.T.) ;
#6562 = ORIENTED_EDGE('',*,*,#5159,.T.) ;
#6563 = ORIENTED_EDGE('',*,*,#5160,.F.) ;
#6564 = ORIENTED_EDGE('',*,*,#5043,.T.) ;
#6565 = ORIENTED_EDGE('',*,*,#5161,.T.) ;
#6566 = ORIENTED_EDGE('',*,*,#5162,.F.) ;
#6567 = ORIENTED_EDGE('',*,*,#5140,.T.) ;
#6568 = ORIENTED_EDGE('',*,*,#5154,.T.) ;
#6569 = ORIENTED_EDGE('',*,*,#5163,.T.) ;
#6570 = ORIENTED_EDGE('',*,*,#5164,.T.) ;
#6571 = ORIENTED_EDGE('',*,*,#5165,.T.) ;
#6572 = ORIENTED_EDGE('',*,*,#5165,.F.) ;
#6573 = ORIENTED_EDGE('',*,*,#5166,.F.) ;
#6574 = ORIENTED_EDGE('',*,*,#5167,.T.) ;
#6575 = ORIENTED_EDGE('',*,*,#5168,.T.) ;
#6576 = ORIENTED_EDGE('',*,*,#5169,.T.) ;
#6577 = ORIENTED_EDGE('',*,*,#5155,.T.) ;
#6578 = ORIENTED_EDGE('',*,*,#5083,.T.) ;
#6579 = ORIENTED_EDGE('',*,*,#5170,.F.) ;
#6580 = ORIENTED_EDGE('',*,*,#5171,.T.) ;
#6581 = ORIENTED_EDGE('',*,*,#5172,.T.) ;
#6582 = ORIENTED_EDGE('',*,*,#5173,.F.) ;
#6583 = ORIENTED_EDGE('',*,*,#5174,.F.) ;
#6584 = ORIENTED_EDGE('',*,*,#5152,.F.) ;
#6585 = ORIENTED_EDGE('',*,*,#5175,.T.) ;
#6586 = ORIENTED_EDGE('',*,*,#5150,.F.) ;
#6587 = ORIENTED_EDGE('',*,*,#5176,.F.) ;
#6588 = ORIENTED_EDGE('',*,*,#5177,.F.) ;
#6589 = ORIENTED_EDGE('',*,*,#5178,.T.) ;
#6590 = ORIENTED_EDGE('',*,*,#5171,.F.) ;
#6591 = ORIENTED_EDGE('',*,*,#5092,.T.) ;
#6592 = ORIENTED_EDGE('',*,*,#5093,.T.) ;
#6593 = ORIENTED_EDGE('',*,*,#5151,.F.) ;
#6594 = ORIENTED_EDGE('',*,*,#5175,.F.) ;
#6595 = ORIENTED_EDGE('',*,*,#5179,.F.) ;
#6596 = ORIENTED_EDGE('',*,*,#5172,.F.) ;
#6597 = ORIENTED_EDGE('',*,*,#5178,.F.) ;
#6598 = ORIENTED_EDGE('',*,*,#5170,.T.) ;
#6599 = ORIENTED_EDGE('',*,*,#5097,.T.) ;
#6600 = ORIENTED_EDGE('',*,*,#5173,.T.) ;
#6601 = ORIENTED_EDGE('',*,*,#5179,.T.) ;
#6602 = ORIENTED_EDGE('',*,*,#5177,.T.) ;
#6603 = ORIENTED_EDGE('',*,*,#5180,.F.) ;
#6604 = ORIENTED_EDGE('',*,*,#5181,.T.) ;
#6605 = ORIENTED_EDGE('',*,*,#5182,.T.) ;
#6606 = ORIENTED_EDGE('',*,*,#5183,.T.) ;
#6607 = ORIENTED_EDGE('',*,*,#5184,.F.) ;
#6608 = ORIENTED_EDGE('',*,*,#5185,.F.) ;
#6609 = ORIENTED_EDGE('',*,*,#5186,.T.) ;
#6610 = ORIENTED_EDGE('',*,*,#5187,.T.) ;
#6611 = ORIENTED_EDGE('',*,*,#5188,.T.) ;
#6612 = ORIENTED_EDGE('',*,*,#5189,.F.) ;
#6613 = ORIENTED_EDGE('',*,*,#5190,.F.) ;
#6614 = ORIENTED_EDGE('',*,*,#5191,.T.) ;
#6615 = ORIENTED_EDGE('',*,*,#5192,.T.) ;
#6616 = ORIENTED_EDGE('',*,*,#5193,.T.) ;
#6617 = ORIENTED_EDGE('',*,*,#5134,.T.) ;
#6618 = ORIENTED_EDGE('',*,*,#5194,.T.) ;
#6619 = ORIENTED_EDGE('',*,*,#5195,.T.) ;
#6620 = ORIENTED_EDGE('',*,*,#5196,.T.) ;
#6621 = ORIENTED_EDGE('',*,*,#5127,.T.) ;
#6622 = ORIENTED_EDGE('',*,*,#5176,.T.) ;
#6623 = ORIENTED_EDGE('',*,*,#5149,.T.) ;
#6624 = ORIENTED_EDGE('',*,*,#5197,.T.) ;
#6625 = ORIENTED_EDGE('',*,*,#5180,.T.) ;
#6626 = ORIENTED_EDGE('',*,*,#5198,.T.) ;
#6627 = ORIENTED_EDGE('',*,*,#5123,.T.) ;
#6628 = ORIENTED_EDGE('',*,*,#5128,.F.) ;
#6629 = ORIENTED_EDGE('',*,*,#5196,.F.) ;
#6630 = ORIENTED_EDGE('',*,*,#5199,.T.) ;
#6631 = ORIENTED_EDGE('',*,*,#5194,.F.) ;
#6632 = ORIENTED_EDGE('',*,*,#5126,.F.) ;
#6633 = ORIENTED_EDGE('',*,*,#5200,.F.) ;
#6634 = ORIENTED_EDGE('',*,*,#5118,.T.) ;
#6635 = ORIENTED_EDGE('',*,*,#5201,.T.) ;
#6636 = ORIENTED_EDGE('',*,*,#5200,.T.) ;
#6637 = ORIENTED_EDGE('',*,*,#5125,.F.) ;
#6638 = ORIENTED_EDGE('',*,*,#5121,.T.) ;
#6639 = ORIENTED_EDGE('',*,*,#5124,.F.) ;
#6640 = ORIENTED_EDGE('',*,*,#5198,.F.) ;
#6641 = ORIENTED_EDGE('',*,*,#5195,.F.) ;
#6642 = ORIENTED_EDGE('',*,*,#5199,.F.) ;
#6643 = ORIENTED_EDGE('',*,*,#5201,.F.) ;
#6644 = ORIENTED_EDGE('',*,*,#5111,.T.) ;
#6645 = ORIENTED_EDGE('',*,*,#5202,.F.) ;
#6646 = ORIENTED_EDGE('',*,*,#5203,.F.) ;
#6647 = ORIENTED_EDGE('',*,*,#5204,.T.) ;
#6648 = ORIENTED_EDGE('',*,*,#5205,.T.) ;
#6649 = ORIENTED_EDGE('',*,*,#5206,.F.) ;
#6650 = ORIENTED_EDGE('',*,*,#5205,.F.) ;
#6651 = ORIENTED_EDGE('',*,*,#5207,.F.) ;
#6652 = ORIENTED_EDGE('',*,*,#5208,.T.) ;
#6653 = ORIENTED_EDGE('',*,*,#5209,.T.) ;
#6654 = ORIENTED_EDGE('',*,*,#5207,.T.) ;
#6655 = ORIENTED_EDGE('',*,*,#5204,.F.) ;
#6656 = ORIENTED_EDGE('',*,*,#5210,.F.) ;
#6657 = ORIENTED_EDGE('',*,*,#5211,.F.) ;
#6658 = ORIENTED_EDGE('',*,*,#5212,.T.) ;
#6659 = ORIENTED_EDGE('',*,*,#5213,.T.) ;
#6660 = ORIENTED_EDGE('',*,*,#5181,.F.) ;
#6661 = ORIENTED_EDGE('',*,*,#5197,.F.) ;
#6662 = ORIENTED_EDGE('',*,*,#5148,.F.) ;
#6663 = ORIENTED_EDGE('',*,*,#5214,.T.) ;
#6664 = ORIENTED_EDGE('',*,*,#5146,.F.) ;
#6665 = ORIENTED_EDGE('',*,*,#5215,.F.) ;
#6666 = ORIENTED_EDGE('',*,*,#5183,.F.) ;
#6667 = ORIENTED_EDGE('',*,*,#5216,.T.) ;
#6668 = ORIENTED_EDGE('',*,*,#5212,.F.) ;
#6669 = ORIENTED_EDGE('',*,*,#5100,.T.) ;
#6670 = ORIENTED_EDGE('',*,*,#5101,.T.) ;
#6671 = ORIENTED_EDGE('',*,*,#5147,.F.) ;
#6672 = ORIENTED_EDGE('',*,*,#5214,.F.) ;
#6673 = ORIENTED_EDGE('',*,*,#5182,.F.) ;
#6674 = ORIENTED_EDGE('',*,*,#5213,.F.) ;
#6675 = ORIENTED_EDGE('',*,*,#5216,.F.) ;
#6676 = ORIENTED_EDGE('',*,*,#5211,.T.) ;
#6677 = ORIENTED_EDGE('',*,*,#5105,.T.) ;
#6678 = ORIENTED_EDGE('',*,*,#5217,.T.) ;
#6679 = ORIENTED_EDGE('',*,*,#5130,.T.) ;
#6680 = ORIENTED_EDGE('',*,*,#5135,.F.) ;
#6681 = ORIENTED_EDGE('',*,*,#5193,.F.) ;
#6682 = ORIENTED_EDGE('',*,*,#5218,.T.) ;
#6683 = ORIENTED_EDGE('',*,*,#5191,.F.) ;
#6684 = ORIENTED_EDGE('',*,*,#5133,.F.) ;
#6685 = ORIENTED_EDGE('',*,*,#5219,.F.) ;
#6686 = ORIENTED_EDGE('',*,*,#5114,.T.) ;
#6687 = ORIENTED_EDGE('',*,*,#5220,.T.) ;
#6688 = ORIENTED_EDGE('',*,*,#5219,.T.) ;
#6689 = ORIENTED_EDGE('',*,*,#5132,.F.) ;
#6690 = ORIENTED_EDGE('',*,*,#5117,.T.) ;
#6691 = ORIENTED_EDGE('',*,*,#5131,.F.) ;
#6692 = ORIENTED_EDGE('',*,*,#5217,.F.) ;
#6693 = ORIENTED_EDGE('',*,*,#5192,.F.) ;
#6694 = ORIENTED_EDGE('',*,*,#5218,.F.) ;
#6695 = ORIENTED_EDGE('',*,*,#5220,.F.) ;
#6696 = ORIENTED_EDGE('',*,*,#5108,.T.) ;
#6697 = ORIENTED_EDGE('',*,*,#5221,.F.) ;
#6698 = ORIENTED_EDGE('',*,*,#5222,.T.) ;
#6699 = ORIENTED_EDGE('',*,*,#5223,.T.) ;
#6700 = ORIENTED_EDGE('',*,*,#5224,.F.) ;
#6701 = ORIENTED_EDGE('',*,*,#5225,.F.) ;
#6702 = ORIENTED_EDGE('',*,*,#5226,.T.) ;
#6703 = ORIENTED_EDGE('',*,*,#5227,.T.) ;
#6704 = ORIENTED_EDGE('',*,*,#5222,.F.) ;
#6705 = ORIENTED_EDGE('',*,*,#5228,.T.) ;
#6706 = ORIENTED_EDGE('',*,*,#5229,.F.) ;
#6707 = ORIENTED_EDGE('',*,*,#5223,.F.) ;
#6708 = ORIENTED_EDGE('',*,*,#5227,.F.) ;
#6709 = ORIENTED_EDGE('',*,*,#5167,.F.) ;
#6710 = ORIENTED_EDGE('',*,*,#5230,.T.) ;
#6711 = ORIENTED_EDGE('',*,*,#5231,.T.) ;
#6712 = ORIENTED_EDGE('',*,*,#5232,.T.) ;
#6713 = ORIENTED_EDGE('',*,*,#5022,.T.) ;
#6714 = ORIENTED_EDGE('',*,*,#5233,.T.) ;
#6715 = ORIENTED_EDGE('',*,*,#5234,.F.) ;
#6716 = ORIENTED_EDGE('',*,*,#5235,.F.) ;
#6717 = ORIENTED_EDGE('',*,*,#5023,.T.) ;
#6718 = ORIENTED_EDGE('',*,*,#5235,.T.) ;
#6719 = ORIENTED_EDGE('',*,*,#5236,.F.) ;
#6720 = ORIENTED_EDGE('',*,*,#5232,.F.) ;
#6721 = ORIENTED_EDGE('',*,*,#5237,.F.) ;
#6722 = ORIENTED_EDGE('',*,*,#5024,.T.) ;
#6723 = ORIENTED_EDGE('',*,*,#5237,.T.) ;
#6724 = ORIENTED_EDGE('',*,*,#5231,.F.) ;
#6725 = ORIENTED_EDGE('',*,*,#5238,.F.) ;
#6726 = ORIENTED_EDGE('',*,*,#5143,.F.) ;
#6727 = ORIENTED_EDGE('',*,*,#5239,.T.) ;
#6728 = ORIENTED_EDGE('',*,*,#5240,.T.) ;
#6729 = ORIENTED_EDGE('',*,*,#5241,.T.) ;
#6730 = ORIENTED_EDGE('',*,*,#5032,.T.) ;
#6731 = ORIENTED_EDGE('',*,*,#5242,.T.) ;
#6732 = ORIENTED_EDGE('',*,*,#5240,.F.) ;
#6733 = ORIENTED_EDGE('',*,*,#5243,.F.) ;
#6734 = ORIENTED_EDGE('',*,*,#5033,.T.) ;
#6735 = ORIENTED_EDGE('',*,*,#5243,.T.) ;
#6736 = ORIENTED_EDGE('',*,*,#5239,.F.) ;
#6737 = ORIENTED_EDGE('',*,*,#5244,.F.) ;
#6738 = ORIENTED_EDGE('',*,*,#5245,.F.) ;
#6739 = ORIENTED_EDGE('',*,*,#5034,.T.) ;
#6740 = ORIENTED_EDGE('',*,*,#5245,.T.) ;
#6741 = ORIENTED_EDGE('',*,*,#5246,.F.) ;
#6742 = ORIENTED_EDGE('',*,*,#5247,.F.) ;
#6743 = ORIENTED_EDGE('',*,*,#5234,.T.) ;
#6744 = ORIENTED_EDGE('',*,*,#5248,.F.) ;
#6745 = ORIENTED_EDGE('',*,*,#5246,.T.) ;
#6746 = ORIENTED_EDGE('',*,*,#5244,.T.) ;
#6747 = ORIENTED_EDGE('',*,*,#5142,.F.) ;
#6748 = ORIENTED_EDGE('',*,*,#5249,.T.) ;
#6749 = ORIENTED_EDGE('',*,*,#5250,.F.) ;
#6750 = ORIENTED_EDGE('',*,*,#5228,.F.) ;
#6751 = ORIENTED_EDGE('',*,*,#5226,.F.) ;
#6752 = ORIENTED_EDGE('',*,*,#5251,.F.) ;
#6753 = ORIENTED_EDGE('',*,*,#5208,.F.) ;
#6754 = ORIENTED_EDGE('',*,*,#5209,.F.) ;
#6755 = ORIENTED_EDGE('',*,*,#5252,.F.) ;
#6756 = ORIENTED_EDGE('',*,*,#5253,.T.) ;
#6757 = ORIENTED_EDGE('',*,*,#5168,.F.) ;
#6758 = ORIENTED_EDGE('',*,*,#5236,.T.) ;
#6759 = ORIENTED_EDGE('',*,*,#5206,.T.) ;
#6760 = ORIENTED_EDGE('',*,*,#5251,.T.) ;
#6761 = ORIENTED_EDGE('',*,*,#5225,.T.) ;
#6762 = ORIENTED_EDGE('',*,*,#5221,.T.) ;
#6763 = ORIENTED_EDGE('',*,*,#5254,.F.) ;
#6764 = ORIENTED_EDGE('',*,*,#5255,.F.) ;
#6765 = ORIENTED_EDGE('',*,*,#5256,.F.) ;
#6766 = ORIENTED_EDGE('',*,*,#5202,.T.) ;
#6767 = ORIENTED_EDGE('',*,*,#5229,.T.) ;
#6768 = ORIENTED_EDGE('',*,*,#5250,.T.) ;
#6769 = ORIENTED_EDGE('',*,*,#5257,.T.) ;
#6770 = ORIENTED_EDGE('',*,*,#5185,.T.) ;
#6771 = ORIENTED_EDGE('',*,*,#5258,.F.) ;
#6772 = ORIENTED_EDGE('',*,*,#5254,.T.) ;
#6773 = ORIENTED_EDGE('',*,*,#5224,.T.) ;
#6774 = ORIENTED_EDGE('',*,*,#5088,.T.) ;
#6775 = ORIENTED_EDGE('',*,*,#5169,.F.) ;
#6776 = ORIENTED_EDGE('',*,*,#5259,.T.) ;
#6777 = ORIENTED_EDGE('',*,*,#5260,.T.) ;
#6778 = ORIENTED_EDGE('',*,*,#5156,.T.) ;
#6779 = ORIENTED_EDGE('',*,*,#5052,.T.) ;
#6780 = ORIENTED_EDGE('',*,*,#5261,.T.) ;
#6781 = ORIENTED_EDGE('',*,*,#5262,.F.) ;
#6782 = ORIENTED_EDGE('',*,*,#5263,.F.) ;
#6783 = ORIENTED_EDGE('',*,*,#5158,.F.) ;
#6784 = ORIENTED_EDGE('',*,*,#5054,.T.) ;
#6785 = ORIENTED_EDGE('',*,*,#5157,.T.) ;
#6786 = ORIENTED_EDGE('',*,*,#5260,.F.) ;
#6787 = ORIENTED_EDGE('',*,*,#5264,.F.) ;
#6788 = ORIENTED_EDGE('',*,*,#5051,.T.) ;
#6789 = ORIENTED_EDGE('',*,*,#5264,.T.) ;
#6790 = ORIENTED_EDGE('',*,*,#5259,.F.) ;
#6791 = ORIENTED_EDGE('',*,*,#5253,.F.) ;
#6792 = ORIENTED_EDGE('',*,*,#5265,.F.) ;
#6793 = ORIENTED_EDGE('',*,*,#5261,.F.) ;
#6794 = ORIENTED_EDGE('',*,*,#5188,.F.) ;
#6795 = ORIENTED_EDGE('',*,*,#5262,.T.) ;
#6796 = ORIENTED_EDGE('',*,*,#5265,.T.) ;
#6797 = ORIENTED_EDGE('',*,*,#5266,.F.) ;
#6798 = ORIENTED_EDGE('',*,*,#5263,.T.) ;
#6799 = ORIENTED_EDGE('',*,*,#5187,.F.) ;
#6800 = ORIENTED_EDGE('',*,*,#5267,.T.) ;
#6801 = ORIENTED_EDGE('',*,*,#5159,.F.) ;
#6802 = ORIENTED_EDGE('',*,*,#5141,.F.) ;
#6803 = ORIENTED_EDGE('',*,*,#5162,.T.) ;
#6804 = ORIENTED_EDGE('',*,*,#5268,.T.) ;
#6805 = ORIENTED_EDGE('',*,*,#5269,.T.) ;
#6806 = ORIENTED_EDGE('',*,*,#5186,.F.) ;
#6807 = ORIENTED_EDGE('',*,*,#5257,.F.) ;
#6808 = ORIENTED_EDGE('',*,*,#5270,.T.) ;
#6809 = ORIENTED_EDGE('',*,*,#5271,.T.) ;
#6810 = ORIENTED_EDGE('',*,*,#5042,.T.) ;
#6811 = ORIENTED_EDGE('',*,*,#5272,.T.) ;
#6812 = ORIENTED_EDGE('',*,*,#5268,.F.) ;
#6813 = ORIENTED_EDGE('',*,*,#5161,.F.) ;
#6814 = ORIENTED_EDGE('',*,*,#5044,.T.) ;
#6815 = ORIENTED_EDGE('',*,*,#5160,.T.) ;
#6816 = ORIENTED_EDGE('',*,*,#5267,.F.) ;
#6817 = ORIENTED_EDGE('',*,*,#5271,.F.) ;
#6818 = ORIENTED_EDGE('',*,*,#5273,.F.) ;
#6819 = ORIENTED_EDGE('',*,*,#5041,.T.) ;
#6820 = ORIENTED_EDGE('',*,*,#5273,.T.) ;
#6821 = ORIENTED_EDGE('',*,*,#5270,.F.) ;
#6822 = ORIENTED_EDGE('',*,*,#5249,.F.) ;
#6823 = ORIENTED_EDGE('',*,*,#5269,.F.) ;
#6824 = ORIENTED_EDGE('',*,*,#5272,.F.) ;
#6825 = ORIENTED_EDGE('',*,*,#5203,.T.) ;
#6826 = ORIENTED_EDGE('',*,*,#5256,.T.) ;
#6827 = ORIENTED_EDGE('',*,*,#5274,.F.) ;
#6828 = ORIENTED_EDGE('',*,*,#5189,.T.) ;
#6829 = ORIENTED_EDGE('',*,*,#5266,.T.) ;
#6830 = ORIENTED_EDGE('',*,*,#5252,.T.) ;
#6831 = ORIENTED_EDGE('',*,*,#5210,.T.) ;
#6832 = ORIENTED_EDGE('',*,*,#5085,.T.) ;
#6833 = ORIENTED_EDGE('',*,*,#5136,.F.) ;
#6834 = ORIENTED_EDGE('',*,*,#5144,.F.) ;
#6835 = ORIENTED_EDGE('',*,*,#5241,.F.) ;
#6836 = ORIENTED_EDGE('',*,*,#5242,.F.) ;
#6837 = ORIENTED_EDGE('',*,*,#5031,.T.) ;
#6838 = ORIENTED_EDGE('',*,*,#5247,.T.) ;
#6839 = ORIENTED_EDGE('',*,*,#5248,.T.) ;
#6840 = ORIENTED_EDGE('',*,*,#5233,.F.) ;
#6841 = ORIENTED_EDGE('',*,*,#5021,.T.) ;
#6842 = ORIENTED_EDGE('',*,*,#5238,.T.) ;
#6843 = ORIENTED_EDGE('',*,*,#5230,.F.) ;
#6844 = ORIENTED_EDGE('',*,*,#5166,.T.) ;
#6845 = ORIENTED_EDGE('',*,*,#5164,.F.) ;
#6846 = ORIENTED_EDGE('',*,*,#5275,.F.) ;
#6847 = ORIENTED_EDGE('',*,*,#5137,.F.) ;
#6848 = ORIENTED_EDGE('',*,*,#5275,.T.) ;
#6849 = ORIENTED_EDGE('',*,*,#5163,.F.) ;
#6850 = ORIENTED_EDGE('',*,*,#5153,.T.) ;
#6851 = ORIENTED_EDGE('',*,*,#5174,.T.) ;
#6852 = ORIENTED_EDGE('',*,*,#5190,.T.) ;
#6853 = ORIENTED_EDGE('',*,*,#5274,.T.) ;
#6854 = ORIENTED_EDGE('',*,*,#5255,.T.) ;
#6855 = ORIENTED_EDGE('',*,*,#5258,.T.) ;
#6856 = ORIENTED_EDGE('',*,*,#5184,.T.) ;
#6857 = ORIENTED_EDGE('',*,*,#5215,.T.) ;
#6858 = ORIENTED_EDGE('',*,*,#5145,.T.) ;
#6859 = ORIENTED_EDGE('',*,*,#5276,.F.) ;
#6860 = ORIENTED_EDGE('',*,*,#5277,.T.) ;
#6861 = ORIENTED_EDGE('',*,*,#5278,.F.) ;
#6862 = ORIENTED_EDGE('',*,*,#5277,.F.) ;
#6863 = ORIENTED_EDGE('',*,*,#5279,.F.) ;
#6864 = ORIENTED_EDGE('',*,*,#5280,.T.) ;
#6865 = ORIENTED_EDGE('',*,*,#5281,.F.) ;
#6866 = ORIENTED_EDGE('',*,*,#5280,.F.) ;
#6867 = ORIENTED_EDGE('',*,*,#5282,.F.) ;
#6868 = ORIENTED_EDGE('',*,*,#5283,.T.) ;
#6869 = ORIENTED_EDGE('',*,*,#5284,.T.) ;
#6870 = ORIENTED_EDGE('',*,*,#5285,.T.) ;
#6871 = ORIENTED_EDGE('',*,*,#5281,.T.) ;
#6872 = ORIENTED_EDGE('',*,*,#5286,.F.) ;
#6873 = ORIENTED_EDGE('',*,*,#5287,.F.) ;
#6874 = ORIENTED_EDGE('',*,*,#5288,.F.) ;
#6875 = ORIENTED_EDGE('',*,*,#5289,.F.) ;
#6876 = ORIENTED_EDGE('',*,*,#5290,.T.) ;
#6877 = ORIENTED_EDGE('',*,*,#5283,.F.) ;
#6878 = ORIENTED_EDGE('',*,*,#5291,.F.) ;
#6879 = ORIENTED_EDGE('',*,*,#5285,.F.) ;
#6880 = ORIENTED_EDGE('',*,*,#5292,.F.) ;
#6881 = ORIENTED_EDGE('',*,*,#5293,.F.) ;
#6882 = ORIENTED_EDGE('',*,*,#5294,.F.) ;
#6883 = ORIENTED_EDGE('',*,*,#5292,.T.) ;
#6884 = ORIENTED_EDGE('',*,*,#5284,.F.) ;
#6885 = ORIENTED_EDGE('',*,*,#5290,.F.) ;
#6886 = ORIENTED_EDGE('',*,*,#5295,.F.) ;
#6887 = ORIENTED_EDGE('',*,*,#5293,.T.) ;
#6888 = ORIENTED_EDGE('',*,*,#5294,.T.) ;
#6889 = ORIENTED_EDGE('',*,*,#5289,.T.) ;
#6890 = ORIENTED_EDGE('',*,*,#5296,.F.) ;
#6891 = ORIENTED_EDGE('',*,*,#5297,.F.) ;
#6892 = ORIENTED_EDGE('',*,*,#5279,.T.) ;
#6893 = ORIENTED_EDGE('',*,*,#5287,.T.) ;
#6894 = ORIENTED_EDGE('',*,*,#5298,.T.) ;
#6895 = ORIENTED_EDGE('',*,*,#5299,.F.) ;
#6896 = ORIENTED_EDGE('',*,*,#5300,.F.) ;
#6897 = ORIENTED_EDGE('',*,*,#5297,.T.) ;
#6898 = ORIENTED_EDGE('',*,*,#5301,.F.) ;
#6899 = ORIENTED_EDGE('',*,*,#5302,.T.) ;
#6900 = ORIENTED_EDGE('',*,*,#5303,.T.) ;
#6901 = ORIENTED_EDGE('',*,*,#5304,.F.) ;
#6902 = ORIENTED_EDGE('',*,*,#5305,.F.) ;
#6903 = ORIENTED_EDGE('',*,*,#5306,.F.) ;
#6904 = ORIENTED_EDGE('',*,*,#5307,.F.) ;
#6905 = ORIENTED_EDGE('',*,*,#5308,.F.) ;
#6906 = ORIENTED_EDGE('',*,*,#5309,.F.) ;
#6907 = ORIENTED_EDGE('',*,*,#5310,.F.) ;
#6908 = ORIENTED_EDGE('',*,*,#5311,.F.) ;
#6909 = ORIENTED_EDGE('',*,*,#5296,.T.) ;
#6910 = ORIENTED_EDGE('',*,*,#5288,.T.) ;
#6911 = ORIENTED_EDGE('',*,*,#5300,.T.) ;
#6912 = ORIENTED_EDGE('',*,*,#5312,.T.) ;
#6913 = ORIENTED_EDGE('',*,*,#5313,.T.) ;
#6914 = ORIENTED_EDGE('',*,*,#5314,.T.) ;
#6915 = ORIENTED_EDGE('',*,*,#5315,.T.) ;
#6916 = ORIENTED_EDGE('',*,*,#5316,.T.) ;
#6917 = ORIENTED_EDGE('',*,*,#5317,.T.) ;
#6918 = ORIENTED_EDGE('',*,*,#5318,.T.) ;
#6919 = ORIENTED_EDGE('',*,*,#5319,.T.) ;
#6920 = ORIENTED_EDGE('',*,*,#5320,.T.) ;
#6921 = ORIENTED_EDGE('',*,*,#5321,.T.) ;
#6922 = ORIENTED_EDGE('',*,*,#5301,.T.) ;
#6923 = ORIENTED_EDGE('',*,*,#5322,.F.) ;
#6924 = ORIENTED_EDGE('',*,*,#5323,.T.) ;
#6925 = ORIENTED_EDGE('',*,*,#5324,.T.) ;
#6926 = ORIENTED_EDGE('',*,*,#5325,.T.) ;
#6927 = ORIENTED_EDGE('',*,*,#5276,.T.) ;
#6928 = ORIENTED_EDGE('',*,*,#5326,.F.) ;
#6929 = ORIENTED_EDGE('',*,*,#5327,.F.) ;
#6930 = ORIENTED_EDGE('',*,*,#5328,.F.) ;
#6931 = ORIENTED_EDGE('',*,*,#5323,.F.) ;
#6932 = ORIENTED_EDGE('',*,*,#5329,.F.) ;
#6933 = ORIENTED_EDGE('',*,*,#5330,.F.) ;
#6934 = ORIENTED_EDGE('',*,*,#5315,.F.) ;
#6935 = ORIENTED_EDGE('',*,*,#5331,.T.) ;
#6936 = ORIENTED_EDGE('',*,*,#5332,.T.) ;
#6937 = ORIENTED_EDGE('',*,*,#5327,.T.) ;
#6938 = ORIENTED_EDGE('',*,*,#5278,.T.) ;
#6939 = ORIENTED_EDGE('',*,*,#5324,.F.) ;
#6940 = ORIENTED_EDGE('',*,*,#5328,.T.) ;
#6941 = ORIENTED_EDGE('',*,*,#5332,.F.) ;
#6942 = ORIENTED_EDGE('',*,*,#5333,.F.) ;
#6943 = ORIENTED_EDGE('',*,*,#5334,.F.) ;
#6944 = ORIENTED_EDGE('',*,*,#5325,.F.) ;
#6945 = ORIENTED_EDGE('',*,*,#5333,.T.) ;
#6946 = ORIENTED_EDGE('',*,*,#5331,.F.) ;
#6947 = ORIENTED_EDGE('',*,*,#5314,.F.) ;
#6948 = ORIENTED_EDGE('',*,*,#5335,.F.) ;
#6949 = ORIENTED_EDGE('',*,*,#5330,.T.) ;
#6950 = ORIENTED_EDGE('',*,*,#5336,.T.) ;
#6951 = ORIENTED_EDGE('',*,*,#5337,.F.) ;
#6952 = ORIENTED_EDGE('',*,*,#5316,.F.) ;
#6953 = ORIENTED_EDGE('',*,*,#5335,.T.) ;
#6954 = ORIENTED_EDGE('',*,*,#5313,.F.) ;
#6955 = ORIENTED_EDGE('',*,*,#5338,.T.) ;
#6956 = ORIENTED_EDGE('',*,*,#5339,.T.) ;
#6957 = ORIENTED_EDGE('',*,*,#5340,.T.) ;
#6958 = ORIENTED_EDGE('',*,*,#5341,.T.) ;
#6959 = ORIENTED_EDGE('',*,*,#5342,.T.) ;
#6960 = ORIENTED_EDGE('',*,*,#5343,.T.) ;
#6961 = ORIENTED_EDGE('',*,*,#5344,.T.) ;
#6962 = ORIENTED_EDGE('',*,*,#5345,.T.) ;
#6963 = ORIENTED_EDGE('',*,*,#5342,.F.) ;
#6964 = ORIENTED_EDGE('',*,*,#5346,.T.) ;
#6965 = ORIENTED_EDGE('',*,*,#5347,.T.) ;
#6966 = ORIENTED_EDGE('',*,*,#5348,.T.) ;
#6967 = ORIENTED_EDGE('',*,*,#5344,.F.) ;
#6968 = ORIENTED_EDGE('',*,*,#5349,.T.) ;
#6969 = ORIENTED_EDGE('',*,*,#5350,.T.) ;
#6970 = ORIENTED_EDGE('',*,*,#5351,.T.) ;
#6971 = ORIENTED_EDGE('',*,*,#5347,.F.) ;
#6972 = ORIENTED_EDGE('',*,*,#5352,.T.) ;
#6973 = ORIENTED_EDGE('',*,*,#5353,.T.) ;
#6974 = ORIENTED_EDGE('',*,*,#5354,.T.) ;
#6975 = ORIENTED_EDGE('',*,*,#5350,.F.) ;
#6976 = ORIENTED_EDGE('',*,*,#5355,.T.) ;
#6977 = ORIENTED_EDGE('',*,*,#5356,.T.) ;
#6978 = ORIENTED_EDGE('',*,*,#5357,.T.) ;
#6979 = ORIENTED_EDGE('',*,*,#5353,.F.) ;
#6980 = ORIENTED_EDGE('',*,*,#5358,.T.) ;
#6981 = ORIENTED_EDGE('',*,*,#5359,.T.) ;
#6982 = ORIENTED_EDGE('',*,*,#5360,.T.) ;
#6983 = ORIENTED_EDGE('',*,*,#5356,.F.) ;
#6984 = ORIENTED_EDGE('',*,*,#5361,.T.) ;
#6985 = ORIENTED_EDGE('',*,*,#5340,.F.) ;
#6986 = ORIENTED_EDGE('',*,*,#5362,.T.) ;
#6987 = ORIENTED_EDGE('',*,*,#5359,.F.) ;
#6988 = ORIENTED_EDGE('',*,*,#5363,.T.) ;
#6989 = ORIENTED_EDGE('',*,*,#5352,.F.) ;
#6990 = ORIENTED_EDGE('',*,*,#5364,.F.) ;
#6991 = ORIENTED_EDGE('',*,*,#5310,.T.) ;
#6992 = ORIENTED_EDGE('',*,*,#5365,.T.) ;
#6993 = ORIENTED_EDGE('',*,*,#5349,.F.) ;
#6994 = ORIENTED_EDGE('',*,*,#5366,.F.) ;
#6995 = ORIENTED_EDGE('',*,*,#5311,.T.) ;
#6996 = ORIENTED_EDGE('',*,*,#5364,.T.) ;
#6997 = ORIENTED_EDGE('',*,*,#5346,.F.) ;
#6998 = ORIENTED_EDGE('',*,*,#5367,.F.) ;
#6999 = ORIENTED_EDGE('',*,*,#5304,.T.) ;
#7000 = ORIENTED_EDGE('',*,*,#5366,.T.) ;
#7001 = ORIENTED_EDGE('',*,*,#5341,.F.) ;
#7002 = ORIENTED_EDGE('',*,*,#5368,.F.) ;
#7003 = ORIENTED_EDGE('',*,*,#5305,.T.) ;
#7004 = ORIENTED_EDGE('',*,*,#5367,.T.) ;
#7005 = ORIENTED_EDGE('',*,*,#5343,.F.) ;
#7006 = ORIENTED_EDGE('',*,*,#5345,.F.) ;
#7007 = ORIENTED_EDGE('',*,*,#5348,.F.) ;
#7008 = ORIENTED_EDGE('',*,*,#5351,.F.) ;
#7009 = ORIENTED_EDGE('',*,*,#5354,.F.) ;
#7010 = ORIENTED_EDGE('',*,*,#5357,.F.) ;
#7011 = ORIENTED_EDGE('',*,*,#5360,.F.) ;
#7012 = ORIENTED_EDGE('',*,*,#5362,.F.) ;
#7013 = ORIENTED_EDGE('',*,*,#5319,.F.) ;
#7014 = ORIENTED_EDGE('',*,*,#5369,.T.) ;
#7015 = ORIENTED_EDGE('',*,*,#5370,.T.) ;
#7016 = ORIENTED_EDGE('',*,*,#5371,.F.) ;
#7017 = ORIENTED_EDGE('',*,*,#5318,.F.) ;
#7018 = ORIENTED_EDGE('',*,*,#5372,.T.) ;
#7019 = ORIENTED_EDGE('',*,*,#5373,.T.) ;
#7020 = ORIENTED_EDGE('',*,*,#5369,.F.) ;
#7021 = ORIENTED_EDGE('',*,*,#5317,.F.) ;
#7022 = ORIENTED_EDGE('',*,*,#5337,.T.) ;
#7023 = ORIENTED_EDGE('',*,*,#5374,.T.) ;
#7024 = ORIENTED_EDGE('',*,*,#5372,.F.) ;
#7025 = ORIENTED_EDGE('',*,*,#5312,.F.) ;
#7026 = ORIENTED_EDGE('',*,*,#5299,.T.) ;
#7027 = ORIENTED_EDGE('',*,*,#5375,.T.) ;
#7028 = ORIENTED_EDGE('',*,*,#5338,.F.) ;
#7029 = ORIENTED_EDGE('',*,*,#5321,.F.) ;
#7030 = ORIENTED_EDGE('',*,*,#5376,.T.) ;
#7031 = ORIENTED_EDGE('',*,*,#5377,.T.) ;
#7032 = ORIENTED_EDGE('',*,*,#5302,.F.) ;
#7033 = ORIENTED_EDGE('',*,*,#5320,.F.) ;
#7034 = ORIENTED_EDGE('',*,*,#5371,.T.) ;
#7035 = ORIENTED_EDGE('',*,*,#5378,.T.) ;
#7036 = ORIENTED_EDGE('',*,*,#5376,.F.) ;
#7037 = ORIENTED_EDGE('',*,*,#5295,.T.) ;
#7038 = ORIENTED_EDGE('',*,*,#5303,.F.) ;
#7039 = ORIENTED_EDGE('',*,*,#5377,.F.) ;
#7040 = ORIENTED_EDGE('',*,*,#5378,.F.) ;
#7041 = ORIENTED_EDGE('',*,*,#5370,.F.) ;
#7042 = ORIENTED_EDGE('',*,*,#5373,.F.) ;
#7043 = ORIENTED_EDGE('',*,*,#5374,.F.) ;
#7044 = ORIENTED_EDGE('',*,*,#5336,.F.) ;
#7045 = ORIENTED_EDGE('',*,*,#5329,.T.) ;
#7046 = ORIENTED_EDGE('',*,*,#5326,.T.) ;
#7047 = ORIENTED_EDGE('',*,*,#5322,.T.) ;
#7048 = ORIENTED_EDGE('',*,*,#5334,.T.) ;
#7049 = ORIENTED_EDGE('',*,*,#5339,.F.) ;
#7050 = ORIENTED_EDGE('',*,*,#5375,.F.) ;
#7051 = ORIENTED_EDGE('',*,*,#5298,.F.) ;
#7052 = ORIENTED_EDGE('',*,*,#5286,.T.) ;
#7053 = ORIENTED_EDGE('',*,*,#5282,.T.) ;
#7054 = ORIENTED_EDGE('',*,*,#5291,.T.) ;
#7055 = ORIENTED_EDGE('',*,*,#5363,.F.) ;
#7056 = ORIENTED_EDGE('',*,*,#5379,.F.) ;
#7057 = ORIENTED_EDGE('',*,*,#5306,.T.) ;
#7058 = ORIENTED_EDGE('',*,*,#5368,.T.) ;
#7059 = ORIENTED_EDGE('',*,*,#5361,.F.) ;
#7060 = ORIENTED_EDGE('',*,*,#5380,.F.) ;
#7061 = ORIENTED_EDGE('',*,*,#5307,.T.) ;
#7062 = ORIENTED_EDGE('',*,*,#5379,.T.) ;
#7063 = ORIENTED_EDGE('',*,*,#5358,.F.) ;
#7064 = ORIENTED_EDGE('',*,*,#5381,.F.) ;
#7065 = ORIENTED_EDGE('',*,*,#5308,.T.) ;
#7066 = ORIENTED_EDGE('',*,*,#5380,.T.) ;
#7067 = ORIENTED_EDGE('',*,*,#5355,.F.) ;
#7068 = ORIENTED_EDGE('',*,*,#5365,.F.) ;
#7069 = ORIENTED_EDGE('',*,*,#5309,.T.) ;
#7070 = ORIENTED_EDGE('',*,*,#5381,.T.) ;
#7071 = ORIENTED_EDGE('',*,*,#5382,.F.) ;
#7072 = ORIENTED_EDGE('',*,*,#5383,.T.) ;
#7073 = ORIENTED_EDGE('',*,*,#5384,.F.) ;
#7074 = ORIENTED_EDGE('',*,*,#5383,.F.) ;
#7075 = ORIENTED_EDGE('',*,*,#5385,.F.) ;
#7076 = ORIENTED_EDGE('',*,*,#5386,.T.) ;
#7077 = ORIENTED_EDGE('',*,*,#5387,.T.) ;
#7078 = ORIENTED_EDGE('',*,*,#5386,.F.) ;
#7079 = ORIENTED_EDGE('',*,*,#5388,.F.) ;
#7080 = ORIENTED_EDGE('',*,*,#5389,.T.) ;
#7081 = ORIENTED_EDGE('',*,*,#5390,.T.) ;
#7082 = ORIENTED_EDGE('',*,*,#5389,.F.) ;
#7083 = ORIENTED_EDGE('',*,*,#5391,.F.) ;
#7084 = ORIENTED_EDGE('',*,*,#5392,.T.) ;
#7085 = ORIENTED_EDGE('',*,*,#5393,.T.) ;
#7086 = ORIENTED_EDGE('',*,*,#5392,.F.) ;
#7087 = ORIENTED_EDGE('',*,*,#5394,.T.) ;
#7088 = ORIENTED_EDGE('',*,*,#5395,.T.) ;
#7089 = ORIENTED_EDGE('',*,*,#5396,.F.) ;
#7090 = ORIENTED_EDGE('',*,*,#5397,.F.) ;
#7091 = ORIENTED_EDGE('',*,*,#5398,.T.) ;
#7092 = ORIENTED_EDGE('',*,*,#5397,.T.) ;
#7093 = ORIENTED_EDGE('',*,*,#5399,.F.) ;
#7094 = ORIENTED_EDGE('',*,*,#5400,.F.) ;
#7095 = ORIENTED_EDGE('',*,*,#5401,.T.) ;
#7096 = ORIENTED_EDGE('',*,*,#5400,.T.) ;
#7097 = ORIENTED_EDGE('',*,*,#5402,.F.) ;
#7098 = ORIENTED_EDGE('',*,*,#5403,.F.) ;
#7099 = ORIENTED_EDGE('',*,*,#5404,.T.) ;
#7100 = ORIENTED_EDGE('',*,*,#5403,.T.) ;
#7101 = ORIENTED_EDGE('',*,*,#5405,.F.) ;
#7102 = ORIENTED_EDGE('',*,*,#5395,.F.) ;
#7103 = ORIENTED_EDGE('',*,*,#5405,.T.) ;
#7104 = ORIENTED_EDGE('',*,*,#5402,.T.) ;
#7105 = ORIENTED_EDGE('',*,*,#5399,.T.) ;
#7106 = ORIENTED_EDGE('',*,*,#5396,.T.) ;
#7107 = ORIENTED_EDGE('',*,*,#5384,.T.) ;
#7108 = ORIENTED_EDGE('',*,*,#5391,.T.) ;
#7109 = ORIENTED_EDGE('',*,*,#5388,.T.) ;
#7110 = ORIENTED_EDGE('',*,*,#5385,.T.) ;
#7111 = ORIENTED_EDGE('',*,*,#5404,.F.) ;
#7112 = ORIENTED_EDGE('',*,*,#5394,.F.) ;
#7113 = ORIENTED_EDGE('',*,*,#5398,.F.) ;
#7114 = ORIENTED_EDGE('',*,*,#5401,.F.) ;
#7115 = ORIENTED_EDGE('',*,*,#5393,.F.) ;
#7116 = ORIENTED_EDGE('',*,*,#5390,.F.) ;
#7117 = ORIENTED_EDGE('',*,*,#5387,.F.) ;
#7118 = ORIENTED_EDGE('',*,*,#5406,.F.) ;
#7119 = ORIENTED_EDGE('',*,*,#5407,.T.) ;
#7120 = ORIENTED_EDGE('',*,*,#5408,.T.) ;
#7121 = ORIENTED_EDGE('',*,*,#5407,.F.) ;
#7122 = ORIENTED_EDGE('',*,*,#5409,.F.) ;
#7123 = ORIENTED_EDGE('',*,*,#5410,.T.) ;
#7124 = ORIENTED_EDGE('',*,*,#5411,.T.) ;
#7125 = ORIENTED_EDGE('',*,*,#5410,.F.) ;
#7126 = ORIENTED_EDGE('',*,*,#5412,.F.) ;
#7127 = ORIENTED_EDGE('',*,*,#5413,.T.) ;
#7128 = ORIENTED_EDGE('',*,*,#5414,.T.) ;
#7129 = ORIENTED_EDGE('',*,*,#5413,.F.) ;
#7130 = ORIENTED_EDGE('',*,*,#5415,.T.) ;
#7131 = ORIENTED_EDGE('',*,*,#5416,.T.) ;
#7132 = ORIENTED_EDGE('',*,*,#5417,.F.) ;
#7133 = ORIENTED_EDGE('',*,*,#5418,.F.) ;
#7134 = ORIENTED_EDGE('',*,*,#5419,.T.) ;
#7135 = ORIENTED_EDGE('',*,*,#5418,.T.) ;
#7136 = ORIENTED_EDGE('',*,*,#5420,.F.) ;
#7137 = ORIENTED_EDGE('',*,*,#5421,.F.) ;
#7138 = ORIENTED_EDGE('',*,*,#5422,.T.) ;
#7139 = ORIENTED_EDGE('',*,*,#5421,.T.) ;
#7140 = ORIENTED_EDGE('',*,*,#5423,.F.) ;
#7141 = ORIENTED_EDGE('',*,*,#5424,.F.) ;
#7142 = ORIENTED_EDGE('',*,*,#5425,.T.) ;
#7143 = ORIENTED_EDGE('',*,*,#5424,.T.) ;
#7144 = ORIENTED_EDGE('',*,*,#5426,.F.) ;
#7145 = ORIENTED_EDGE('',*,*,#5416,.F.) ;
#7146 = ORIENTED_EDGE('',*,*,#5426,.T.) ;
#7147 = ORIENTED_EDGE('',*,*,#5423,.T.) ;
#7148 = ORIENTED_EDGE('',*,*,#5420,.T.) ;
#7149 = ORIENTED_EDGE('',*,*,#5417,.T.) ;
#7150 = ORIENTED_EDGE('',*,*,#5412,.T.) ;
#7151 = ORIENTED_EDGE('',*,*,#5409,.T.) ;
#7152 = ORIENTED_EDGE('',*,*,#5406,.T.) ;
#7153 = ORIENTED_EDGE('',*,*,#5425,.F.) ;
#7154 = ORIENTED_EDGE('',*,*,#5415,.F.) ;
#7155 = ORIENTED_EDGE('',*,*,#5419,.F.) ;
#7156 = ORIENTED_EDGE('',*,*,#5422,.F.) ;
#7157 = ORIENTED_EDGE('',*,*,#5382,.T.) ;
#7158 = ORIENTED_EDGE('',*,*,#5414,.F.) ;
#7159 = ORIENTED_EDGE('',*,*,#5411,.F.) ;
#7160 = ORIENTED_EDGE('',*,*,#5408,.F.) ;
#7161 = ORIENTED_EDGE('',*,*,#5427,.F.) ;
#7162 = ORIENTED_EDGE('',*,*,#5428,.T.) ;
#7163 = ORIENTED_EDGE('',*,*,#5429,.F.) ;
#7164 = ORIENTED_EDGE('',*,*,#5428,.F.) ;
#7165 = ORIENTED_EDGE('',*,*,#5430,.F.) ;
#7166 = ORIENTED_EDGE('',*,*,#5431,.T.) ;
#7167 = ORIENTED_EDGE('',*,*,#5432,.F.) ;
#7168 = ORIENTED_EDGE('',*,*,#5431,.F.) ;
#7169 = ORIENTED_EDGE('',*,*,#5433,.F.) ;
#7170 = ORIENTED_EDGE('',*,*,#5434,.T.) ;
#7171 = ORIENTED_EDGE('',*,*,#5435,.T.) ;
#7172 = ORIENTED_EDGE('',*,*,#5434,.F.) ;
#7173 = ORIENTED_EDGE('',*,*,#5436,.F.) ;
#7174 = ORIENTED_EDGE('',*,*,#5437,.T.) ;
#7175 = ORIENTED_EDGE('',*,*,#5438,.T.) ;
#7176 = ORIENTED_EDGE('',*,*,#5437,.F.) ;
#7177 = ORIENTED_EDGE('',*,*,#5439,.F.) ;
#7178 = ORIENTED_EDGE('',*,*,#5440,.T.) ;
#7179 = ORIENTED_EDGE('',*,*,#5441,.T.) ;
#7180 = ORIENTED_EDGE('',*,*,#5440,.F.) ;
#7181 = ORIENTED_EDGE('',*,*,#5442,.T.) ;
#7182 = ORIENTED_EDGE('',*,*,#5443,.T.) ;
#7183 = ORIENTED_EDGE('',*,*,#5444,.F.) ;
#7184 = ORIENTED_EDGE('',*,*,#5445,.F.) ;
#7185 = ORIENTED_EDGE('',*,*,#5446,.T.) ;
#7186 = ORIENTED_EDGE('',*,*,#5445,.T.) ;
#7187 = ORIENTED_EDGE('',*,*,#5447,.F.) ;
#7188 = ORIENTED_EDGE('',*,*,#5448,.F.) ;
#7189 = ORIENTED_EDGE('',*,*,#5449,.T.) ;
#7190 = ORIENTED_EDGE('',*,*,#5448,.T.) ;
#7191 = ORIENTED_EDGE('',*,*,#5450,.F.) ;
#7192 = ORIENTED_EDGE('',*,*,#5451,.F.) ;
#7193 = ORIENTED_EDGE('',*,*,#5452,.T.) ;
#7194 = ORIENTED_EDGE('',*,*,#5451,.T.) ;
#7195 = ORIENTED_EDGE('',*,*,#5453,.F.) ;
#7196 = ORIENTED_EDGE('',*,*,#5443,.F.) ;
#7197 = ORIENTED_EDGE('',*,*,#5453,.T.) ;
#7198 = ORIENTED_EDGE('',*,*,#5450,.T.) ;
#7199 = ORIENTED_EDGE('',*,*,#5447,.T.) ;
#7200 = ORIENTED_EDGE('',*,*,#5444,.T.) ;
#7201 = ORIENTED_EDGE('',*,*,#5429,.T.) ;
#7202 = ORIENTED_EDGE('',*,*,#5432,.T.) ;
#7203 = ORIENTED_EDGE('',*,*,#5439,.T.) ;
#7204 = ORIENTED_EDGE('',*,*,#5436,.T.) ;
#7205 = ORIENTED_EDGE('',*,*,#5433,.T.) ;
#7206 = ORIENTED_EDGE('',*,*,#5452,.F.) ;
#7207 = ORIENTED_EDGE('',*,*,#5442,.F.) ;
#7208 = ORIENTED_EDGE('',*,*,#5446,.F.) ;
#7209 = ORIENTED_EDGE('',*,*,#5449,.F.) ;
#7210 = ORIENTED_EDGE('',*,*,#5441,.F.) ;
#7211 = ORIENTED_EDGE('',*,*,#5438,.F.) ;
#7212 = ORIENTED_EDGE('',*,*,#5435,.F.) ;
#7213 = ORIENTED_EDGE('',*,*,#5454,.F.) ;
#7214 = ORIENTED_EDGE('',*,*,#5455,.T.) ;
#7215 = ORIENTED_EDGE('',*,*,#5456,.T.) ;
#7216 = ORIENTED_EDGE('',*,*,#5455,.F.) ;
#7217 = ORIENTED_EDGE('',*,*,#5457,.F.) ;
#7218 = ORIENTED_EDGE('',*,*,#5458,.T.) ;
#7219 = ORIENTED_EDGE('',*,*,#5459,.T.) ;
#7220 = ORIENTED_EDGE('',*,*,#5458,.F.) ;
#7221 = ORIENTED_EDGE('',*,*,#5460,.F.) ;
#7222 = ORIENTED_EDGE('',*,*,#5461,.T.) ;
#7223 = ORIENTED_EDGE('',*,*,#5462,.T.) ;
#7224 = ORIENTED_EDGE('',*,*,#5461,.F.) ;
#7225 = ORIENTED_EDGE('',*,*,#5463,.T.) ;
#7226 = ORIENTED_EDGE('',*,*,#5464,.T.) ;
#7227 = ORIENTED_EDGE('',*,*,#5465,.F.) ;
#7228 = ORIENTED_EDGE('',*,*,#5466,.F.) ;
#7229 = ORIENTED_EDGE('',*,*,#5467,.T.) ;
#7230 = ORIENTED_EDGE('',*,*,#5466,.T.) ;
#7231 = ORIENTED_EDGE('',*,*,#5468,.F.) ;
#7232 = ORIENTED_EDGE('',*,*,#5469,.F.) ;
#7233 = ORIENTED_EDGE('',*,*,#5470,.T.) ;
#7234 = ORIENTED_EDGE('',*,*,#5469,.T.) ;
#7235 = ORIENTED_EDGE('',*,*,#5471,.F.) ;
#7236 = ORIENTED_EDGE('',*,*,#5472,.F.) ;
#7237 = ORIENTED_EDGE('',*,*,#5473,.T.) ;
#7238 = ORIENTED_EDGE('',*,*,#5472,.T.) ;
#7239 = ORIENTED_EDGE('',*,*,#5474,.F.) ;
#7240 = ORIENTED_EDGE('',*,*,#5464,.F.) ;
#7241 = ORIENTED_EDGE('',*,*,#5474,.T.) ;
#7242 = ORIENTED_EDGE('',*,*,#5471,.T.) ;
#7243 = ORIENTED_EDGE('',*,*,#5468,.T.) ;
#7244 = ORIENTED_EDGE('',*,*,#5465,.T.) ;
#7245 = ORIENTED_EDGE('',*,*,#5460,.T.) ;
#7246 = ORIENTED_EDGE('',*,*,#5457,.T.) ;
#7247 = ORIENTED_EDGE('',*,*,#5454,.T.) ;
#7248 = ORIENTED_EDGE('',*,*,#5473,.F.) ;
#7249 = ORIENTED_EDGE('',*,*,#5463,.F.) ;
#7250 = ORIENTED_EDGE('',*,*,#5467,.F.) ;
#7251 = ORIENTED_EDGE('',*,*,#5470,.F.) ;
#7252 = ORIENTED_EDGE('',*,*,#5427,.T.) ;
#7253 = ORIENTED_EDGE('',*,*,#5430,.T.) ;
#7254 = ORIENTED_EDGE('',*,*,#5462,.F.) ;
#7255 = ORIENTED_EDGE('',*,*,#5459,.F.) ;
#7256 = ORIENTED_EDGE('',*,*,#5456,.F.) ;
#7257 = ORIENTED_EDGE('',*,*,#5475,.T.) ;
#7258 = ORIENTED_EDGE('',*,*,#5476,.T.) ;
#7259 = ORIENTED_EDGE('',*,*,#5477,.T.) ;
#7260 = ORIENTED_EDGE('',*,*,#5478,.F.) ;
#7261 = ORIENTED_EDGE('',*,*,#5479,.F.) ;
#7262 = ORIENTED_EDGE('',*,*,#5480,.T.) ;
#7263 = ORIENTED_EDGE('',*,*,#5481,.T.) ;
#7264 = ORIENTED_EDGE('',*,*,#5482,.T.) ;
#7265 = ORIENTED_EDGE('',*,*,#5475,.F.) ;
#7266 = ORIENTED_EDGE('',*,*,#5483,.T.) ;
#7267 = ORIENTED_EDGE('',*,*,#5484,.F.) ;
#7268 = ORIENTED_EDGE('',*,*,#5485,.T.) ;
#7269 = ORIENTED_EDGE('',*,*,#5486,.F.) ;
#7270 = ORIENTED_EDGE('',*,*,#5485,.F.) ;
#7271 = ORIENTED_EDGE('',*,*,#5487,.F.) ;
#7272 = ORIENTED_EDGE('',*,*,#5487,.T.) ;
#7273 = ORIENTED_EDGE('',*,*,#5488,.T.) ;
#7274 = ORIENTED_EDGE('',*,*,#5489,.F.) ;
#7275 = ORIENTED_EDGE('',*,*,#5488,.F.) ;
#7276 = ORIENTED_EDGE('',*,*,#5489,.T.) ;
#7277 = ORIENTED_EDGE('',*,*,#5490,.F.) ;
#7278 = ORIENTED_EDGE('',*,*,#5490,.T.) ;
#7279 = ORIENTED_EDGE('',*,*,#5491,.T.) ;
#7280 = ORIENTED_EDGE('',*,*,#5492,.F.) ;
#7281 = ORIENTED_EDGE('',*,*,#5491,.F.) ;
#7282 = ORIENTED_EDGE('',*,*,#5493,.F.) ;
#7283 = ORIENTED_EDGE('',*,*,#5492,.T.) ;
#7284 = ORIENTED_EDGE('',*,*,#5494,.F.) ;
#7285 = ORIENTED_EDGE('',*,*,#5495,.T.) ;
#7286 = ORIENTED_EDGE('',*,*,#5493,.T.) ;
#7287 = ORIENTED_EDGE('',*,*,#5495,.F.) ;
#7288 = ORIENTED_EDGE('',*,*,#5494,.T.) ;
#7289 = ORIENTED_EDGE('',*,*,#5496,.F.) ;
#7290 = ORIENTED_EDGE('',*,*,#5480,.F.) ;
#7291 = ORIENTED_EDGE('',*,*,#5497,.F.) ;
#7292 = ORIENTED_EDGE('',*,*,#5483,.F.) ;
#7293 = ORIENTED_EDGE('',*,*,#5477,.F.) ;
#7294 = ORIENTED_EDGE('',*,*,#5481,.F.) ;
#7295 = ORIENTED_EDGE('',*,*,#5498,.T.) ;
#7296 = ORIENTED_EDGE('',*,*,#5496,.T.) ;
#7297 = ORIENTED_EDGE('',*,*,#5498,.F.) ;
#7298 = ORIENTED_EDGE('',*,*,#5478,.T.) ;
#7299 = ORIENTED_EDGE('',*,*,#5497,.T.) ;
#7300 = ORIENTED_EDGE('',*,*,#5499,.F.) ;
#7301 = ORIENTED_EDGE('',*,*,#5479,.T.) ;
#7302 = ORIENTED_EDGE('',*,*,#5499,.T.) ;
#7303 = ORIENTED_EDGE('',*,*,#5486,.T.) ;
#7304 = ORIENTED_EDGE('',*,*,#5482,.F.) ;
#7305 = ORIENTED_EDGE('',*,*,#5476,.F.) ;
#7306 = ORIENTED_EDGE('',*,*,#5484,.T.) ;
#7307 = ORIENTED_EDGE('',*,*,#5500,.F.) ;
#7308 = ORIENTED_EDGE('',*,*,#5501,.F.) ;
#7309 = ORIENTED_EDGE('',*,*,#5502,.F.) ;
#7310 = ORIENTED_EDGE('',*,*,#5503,.F.) ;
#7311 = ORIENTED_EDGE('',*,*,#5504,.F.) ;
#7312 = ORIENTED_EDGE('',*,*,#5505,.T.) ;
#7313 = ORIENTED_EDGE('',*,*,#5506,.F.) ;
#7314 = ORIENTED_EDGE('',*,*,#5507,.T.) ;
#7315 = ORIENTED_EDGE('',*,*,#5508,.F.) ;
#7316 = ORIENTED_EDGE('',*,*,#5507,.F.) ;
#7317 = ORIENTED_EDGE('',*,*,#5500,.T.) ;
#7318 = ORIENTED_EDGE('',*,*,#5509,.T.) ;
#7319 = ORIENTED_EDGE('',*,*,#5510,.F.) ;
#7320 = ORIENTED_EDGE('',*,*,#5511,.F.) ;
#7321 = ORIENTED_EDGE('',*,*,#5512,.F.) ;
#7322 = ORIENTED_EDGE('',*,*,#5513,.F.) ;
#7323 = ORIENTED_EDGE('',*,*,#5501,.T.) ;
#7324 = ORIENTED_EDGE('',*,*,#5513,.T.) ;
#7325 = ORIENTED_EDGE('',*,*,#5508,.T.) ;
#7326 = ORIENTED_EDGE('',*,*,#5505,.F.) ;
#7327 = ORIENTED_EDGE('',*,*,#5509,.F.) ;
#7328 = ORIENTED_EDGE('',*,*,#5506,.T.) ;
#7329 = ORIENTED_EDGE('',*,*,#5511,.T.) ;
#7330 = ORIENTED_EDGE('',*,*,#5514,.F.) ;
#7331 = ORIENTED_EDGE('',*,*,#5515,.F.) ;
#7332 = ORIENTED_EDGE('',*,*,#5503,.T.) ;
#7333 = ORIENTED_EDGE('',*,*,#5516,.F.) ;
#7334 = ORIENTED_EDGE('',*,*,#5517,.F.) ;
#7335 = ORIENTED_EDGE('',*,*,#5518,.T.) ;
#7336 = ORIENTED_EDGE('',*,*,#5514,.T.) ;
#7337 = ORIENTED_EDGE('',*,*,#5510,.T.) ;
#7338 = ORIENTED_EDGE('',*,*,#5504,.T.) ;
#7339 = ORIENTED_EDGE('',*,*,#5516,.T.) ;
#7340 = ORIENTED_EDGE('',*,*,#5502,.T.) ;
#7341 = ORIENTED_EDGE('',*,*,#5512,.T.) ;
#7342 = ORIENTED_EDGE('',*,*,#5515,.T.) ;
#7343 = ORIENTED_EDGE('',*,*,#5518,.F.) ;
#7344 = ORIENTED_EDGE('',*,*,#5519,.F.) ;
#7345 = ORIENTED_EDGE('',*,*,#5517,.T.) ;
#7346 = ORIENTED_EDGE('',*,*,#5520,.F.) ;
#7347 = ORIENTED_EDGE('',*,*,#5521,.T.) ;
#7348 = ORIENTED_EDGE('',*,*,#5519,.T.) ;
#7349 = ORIENTED_EDGE('',*,*,#5521,.F.) ;
#7350 = ORIENTED_EDGE('',*,*,#5520,.T.) ;
#7351 = ORIENTED_EDGE('',*,*,#5522,.F.) ;
#7352 = ORIENTED_EDGE('',*,*,#5523,.F.) ;
#7353 = ORIENTED_EDGE('',*,*,#5524,.F.) ;
#7354 = ORIENTED_EDGE('',*,*,#5525,.F.) ;
#7355 = ORIENTED_EDGE('',*,*,#5523,.T.) ;
#7356 = ORIENTED_EDGE('',*,*,#5526,.T.) ;
#7357 = ORIENTED_EDGE('',*,*,#5527,.T.) ;
#7358 = ORIENTED_EDGE('',*,*,#5528,.T.) ;
#7359 = ORIENTED_EDGE('',*,*,#5529,.F.) ;
#7360 = ORIENTED_EDGE('',*,*,#5530,.F.) ;
#7361 = ORIENTED_EDGE('',*,*,#5531,.F.) ;
#7362 = ORIENTED_EDGE('',*,*,#5532,.T.) ;
#7363 = ORIENTED_EDGE('',*,*,#5533,.T.) ;
#7364 = ORIENTED_EDGE('',*,*,#5522,.T.) ;
#7365 = ORIENTED_EDGE('',*,*,#5534,.F.) ;
#7366 = ORIENTED_EDGE('',*,*,#5535,.F.) ;
#7367 = ORIENTED_EDGE('',*,*,#5526,.F.) ;
#7368 = ORIENTED_EDGE('',*,*,#5524,.T.) ;
#7369 = ORIENTED_EDGE('',*,*,#5533,.F.) ;
#7370 = ORIENTED_EDGE('',*,*,#5536,.T.) ;
#7371 = ORIENTED_EDGE('',*,*,#5537,.F.) ;
#7372 = ORIENTED_EDGE('',*,*,#5538,.F.) ;
#7373 = ORIENTED_EDGE('',*,*,#5539,.T.) ;
#7374 = ORIENTED_EDGE('',*,*,#5540,.F.) ;
#7375 = ORIENTED_EDGE('',*,*,#5541,.F.) ;
#7376 = ORIENTED_EDGE('',*,*,#5542,.F.) ;
#7377 = ORIENTED_EDGE('',*,*,#5536,.F.) ;
#7378 = ORIENTED_EDGE('',*,*,#5532,.F.) ;
#7379 = ORIENTED_EDGE('',*,*,#5543,.F.) ;
#7380 = ORIENTED_EDGE('',*,*,#5528,.F.) ;
#7381 = ORIENTED_EDGE('',*,*,#5544,.T.) ;
#7382 = ORIENTED_EDGE('',*,*,#5545,.F.) ;
#7383 = ORIENTED_EDGE('',*,*,#5539,.F.) ;
#7384 = ORIENTED_EDGE('',*,*,#5546,.F.) ;
#7385 = ORIENTED_EDGE('',*,*,#5547,.F.) ;
#7386 = ORIENTED_EDGE('',*,*,#5527,.F.) ;
#7387 = ORIENTED_EDGE('',*,*,#5535,.T.) ;
#7388 = ORIENTED_EDGE('',*,*,#5548,.F.) ;
#7389 = ORIENTED_EDGE('',*,*,#5544,.F.) ;
#7390 = ORIENTED_EDGE('',*,*,#5525,.T.) ;
#7391 = ORIENTED_EDGE('',*,*,#5537,.T.) ;
#7392 = ORIENTED_EDGE('',*,*,#5542,.T.) ;
#7393 = ORIENTED_EDGE('',*,*,#5540,.T.) ;
#7394 = ORIENTED_EDGE('',*,*,#5545,.T.) ;
#7395 = ORIENTED_EDGE('',*,*,#5548,.T.) ;
#7396 = ORIENTED_EDGE('',*,*,#5534,.T.) ;
#7397 = ORIENTED_EDGE('',*,*,#5529,.T.) ;
#7398 = ORIENTED_EDGE('',*,*,#5543,.T.) ;
#7399 = ORIENTED_EDGE('',*,*,#5549,.T.) ;
#7400 = ORIENTED_EDGE('',*,*,#5530,.T.) ;
#7401 = ORIENTED_EDGE('',*,*,#5549,.F.) ;
#7402 = ORIENTED_EDGE('',*,*,#5547,.T.) ;
#7403 = ORIENTED_EDGE('',*,*,#5550,.T.) ;
#7404 = ORIENTED_EDGE('',*,*,#5551,.T.) ;
#7405 = ORIENTED_EDGE('',*,*,#5552,.F.) ;
#7406 = ORIENTED_EDGE('',*,*,#5553,.F.) ;
#7407 = ORIENTED_EDGE('',*,*,#5531,.T.) ;
#7408 = ORIENTED_EDGE('',*,*,#5551,.F.) ;
#7409 = ORIENTED_EDGE('',*,*,#5554,.T.) ;
#7410 = ORIENTED_EDGE('',*,*,#5555,.F.) ;
#7411 = ORIENTED_EDGE('',*,*,#5556,.F.) ;
#7412 = ORIENTED_EDGE('',*,*,#5553,.T.) ;
#7413 = ORIENTED_EDGE('',*,*,#5557,.F.) ;
#7414 = ORIENTED_EDGE('',*,*,#5558,.F.) ;
#7415 = ORIENTED_EDGE('',*,*,#5554,.F.) ;
#7416 = ORIENTED_EDGE('',*,*,#5550,.F.) ;
#7417 = ORIENTED_EDGE('',*,*,#5546,.T.) ;
#7418 = ORIENTED_EDGE('',*,*,#5538,.T.) ;
#7419 = ORIENTED_EDGE('',*,*,#5541,.T.) ;
#7420 = ORIENTED_EDGE('',*,*,#5555,.T.) ;
#7421 = ORIENTED_EDGE('',*,*,#5558,.T.) ;
#7422 = ORIENTED_EDGE('',*,*,#5559,.T.) ;
#7423 = ORIENTED_EDGE('',*,*,#5560,.T.) ;
#7424 = ORIENTED_EDGE('',*,*,#5561,.T.) ;
#7425 = ORIENTED_EDGE('',*,*,#5562,.T.) ;
#7426 = ORIENTED_EDGE('',*,*,#5563,.T.) ;
#7427 = ORIENTED_EDGE('',*,*,#5564,.T.) ;
#7428 = ORIENTED_EDGE('',*,*,#5565,.T.) ;
#7429 = ORIENTED_EDGE('',*,*,#5560,.F.) ;
#7430 = ORIENTED_EDGE('',*,*,#5566,.F.) ;
#7431 = ORIENTED_EDGE('',*,*,#5556,.T.) ;
#7432 = ORIENTED_EDGE('',*,*,#5563,.F.) ;
#7433 = ORIENTED_EDGE('',*,*,#5567,.F.) ;
#7434 = ORIENTED_EDGE('',*,*,#5568,.T.) ;
#7435 = ORIENTED_EDGE('',*,*,#5566,.T.) ;
#7436 = ORIENTED_EDGE('',*,*,#5559,.F.) ;
#7437 = ORIENTED_EDGE('',*,*,#5557,.T.) ;
#7438 = ORIENTED_EDGE('',*,*,#5552,.T.) ;
#7439 = ORIENTED_EDGE('',*,*,#5569,.T.) ;
#7440 = ORIENTED_EDGE('',*,*,#5567,.T.) ;
#7441 = ORIENTED_EDGE('',*,*,#5562,.F.) ;
#7442 = ORIENTED_EDGE('',*,*,#5570,.F.) ;
#7443 = ORIENTED_EDGE('',*,*,#5571,.T.) ;
#7444 = ORIENTED_EDGE('',*,*,#5570,.T.) ;
#7445 = ORIENTED_EDGE('',*,*,#5561,.F.) ;
#7446 = ORIENTED_EDGE('',*,*,#5565,.F.) ;
#7447 = ORIENTED_EDGE('',*,*,#5571,.F.) ;
#7448 = ORIENTED_EDGE('',*,*,#5564,.F.) ;
#7449 = ORIENTED_EDGE('',*,*,#5568,.F.) ;
#7450 = ORIENTED_EDGE('',*,*,#5569,.F.) ;
#7451 = ORIENTED_EDGE('',*,*,#5572,.T.) ;
#7452 = ORIENTED_EDGE('',*,*,#5573,.T.) ;
#7453 = ORIENTED_EDGE('',*,*,#5574,.F.) ;
#7454 = ORIENTED_EDGE('',*,*,#5575,.F.) ;
#7455 = ORIENTED_EDGE('',*,*,#5576,.T.) ;
#7456 = ORIENTED_EDGE('',*,*,#5575,.T.) ;
#7457 = ORIENTED_EDGE('',*,*,#5577,.F.) ;
#7458 = ORIENTED_EDGE('',*,*,#5578,.F.) ;
#7459 = ORIENTED_EDGE('',*,*,#5579,.T.) ;
#7460 = ORIENTED_EDGE('',*,*,#5580,.T.) ;
#7461 = ORIENTED_EDGE('',*,*,#5581,.F.) ;
#7462 = ORIENTED_EDGE('',*,*,#5573,.F.) ;
#7463 = ORIENTED_EDGE('',*,*,#5582,.F.) ;
#7464 = ORIENTED_EDGE('',*,*,#5583,.T.) ;
#7465 = ORIENTED_EDGE('',*,*,#5577,.T.) ;
#7466 = ORIENTED_EDGE('',*,*,#5574,.T.) ;
#7467 = ORIENTED_EDGE('',*,*,#5581,.T.) ;
#7468 = ORIENTED_EDGE('',*,*,#5584,.T.) ;
#7469 = ORIENTED_EDGE('',*,*,#5585,.F.) ;
#7470 = ORIENTED_EDGE('',*,*,#5586,.F.) ;
#7471 = ORIENTED_EDGE('',*,*,#5579,.F.) ;
#7472 = ORIENTED_EDGE('',*,*,#5572,.F.) ;
#7473 = ORIENTED_EDGE('',*,*,#5576,.F.) ;
#7474 = ORIENTED_EDGE('',*,*,#5587,.F.) ;
#7475 = ORIENTED_EDGE('',*,*,#5586,.T.) ;
#7476 = ORIENTED_EDGE('',*,*,#5588,.T.) ;
#7477 = ORIENTED_EDGE('',*,*,#5589,.T.) ;
#7478 = ORIENTED_EDGE('',*,*,#5590,.T.) ;
#7479 = ORIENTED_EDGE('',*,*,#5591,.T.) ;
#7480 = ORIENTED_EDGE('',*,*,#5592,.T.) ;
#7481 = ORIENTED_EDGE('',*,*,#5585,.T.) ;
#7482 = ORIENTED_EDGE('',*,*,#5593,.T.) ;
#7483 = ORIENTED_EDGE('',*,*,#5594,.T.) ;
#7484 = ORIENTED_EDGE('',*,*,#5588,.F.) ;
#7485 = ORIENTED_EDGE('',*,*,#5592,.F.) ;
#7486 = ORIENTED_EDGE('',*,*,#5595,.T.) ;
#7487 = ORIENTED_EDGE('',*,*,#5596,.T.) ;
#7488 = ORIENTED_EDGE('',*,*,#5595,.F.) ;
#7489 = ORIENTED_EDGE('',*,*,#5582,.T.) ;
#7490 = ORIENTED_EDGE('',*,*,#5591,.F.) ;
#7491 = ORIENTED_EDGE('',*,*,#5597,.F.) ;
#7492 = ORIENTED_EDGE('',*,*,#5598,.T.) ;
#7493 = ORIENTED_EDGE('',*,*,#5599,.T.) ;
#7494 = ORIENTED_EDGE('',*,*,#5597,.T.) ;
#7495 = ORIENTED_EDGE('',*,*,#5590,.F.) ;
#7496 = ORIENTED_EDGE('',*,*,#5600,.F.) ;
#7497 = ORIENTED_EDGE('',*,*,#5601,.T.) ;
#7498 = ORIENTED_EDGE('',*,*,#5600,.T.) ;
#7499 = ORIENTED_EDGE('',*,*,#5589,.F.) ;
#7500 = ORIENTED_EDGE('',*,*,#5594,.F.) ;
#7501 = ORIENTED_EDGE('',*,*,#5598,.F.) ;
#7502 = ORIENTED_EDGE('',*,*,#5599,.F.) ;
#7503 = ORIENTED_EDGE('',*,*,#5601,.F.) ;
#7504 = ORIENTED_EDGE('',*,*,#5593,.F.) ;
#7505 = ORIENTED_EDGE('',*,*,#5584,.F.) ;
#7506 = ORIENTED_EDGE('',*,*,#5580,.F.) ;
#7507 = ORIENTED_EDGE('',*,*,#5587,.T.) ;
#7508 = ORIENTED_EDGE('',*,*,#5578,.T.) ;
#7509 = ORIENTED_EDGE('',*,*,#5583,.F.) ;
#7510 = ORIENTED_EDGE('',*,*,#5596,.F.) ;
#7511 = ORIENTED_EDGE('',*,*,#5602,.F.) ;
#7512 = ORIENTED_EDGE('',*,*,#5603,.F.) ;
#7513 = ORIENTED_EDGE('',*,*,#5604,.T.) ;
#7514 = ORIENTED_EDGE('',*,*,#5605,.F.) ;
#7515 = ORIENTED_EDGE('',*,*,#5606,.F.) ;
#7516 = ORIENTED_EDGE('',*,*,#5604,.F.) ;
#7517 = ORIENTED_EDGE('',*,*,#5607,.F.) ;
#7518 = ORIENTED_EDGE('',*,*,#5608,.T.) ;
#7519 = ORIENTED_EDGE('',*,*,#5609,.F.) ;
#7520 = ORIENTED_EDGE('',*,*,#5610,.F.) ;
#7521 = ORIENTED_EDGE('',*,*,#5608,.F.) ;
#7522 = ORIENTED_EDGE('',*,*,#5611,.F.) ;
#7523 = ORIENTED_EDGE('',*,*,#5612,.F.) ;
#7524 = ORIENTED_EDGE('',*,*,#5613,.T.) ;
#7525 = ORIENTED_EDGE('',*,*,#5614,.F.) ;
#7526 = ORIENTED_EDGE('',*,*,#5613,.F.) ;
#7527 = ORIENTED_EDGE('',*,*,#5615,.F.) ;
#7528 = ORIENTED_EDGE('',*,*,#5616,.T.) ;
#7529 = ORIENTED_EDGE('',*,*,#5617,.T.) ;
#7530 = ORIENTED_EDGE('',*,*,#5618,.T.) ;
#7531 = ORIENTED_EDGE('',*,*,#5619,.T.) ;
#7532 = ORIENTED_EDGE('',*,*,#5620,.T.) ;
#7533 = ORIENTED_EDGE('',*,*,#5621,.F.) ;
#7534 = ORIENTED_EDGE('',*,*,#5622,.T.) ;
#7535 = ORIENTED_EDGE('',*,*,#5623,.T.) ;
#7536 = ORIENTED_EDGE('',*,*,#5616,.F.) ;
#7537 = ORIENTED_EDGE('',*,*,#5624,.T.) ;
#7538 = ORIENTED_EDGE('',*,*,#5625,.T.) ;
#7539 = ORIENTED_EDGE('',*,*,#5619,.F.) ;
#7540 = ORIENTED_EDGE('',*,*,#5626,.F.) ;
#7541 = ORIENTED_EDGE('',*,*,#5614,.T.) ;
#7542 = ORIENTED_EDGE('',*,*,#5627,.T.) ;
#7543 = ORIENTED_EDGE('',*,*,#5626,.T.) ;
#7544 = ORIENTED_EDGE('',*,*,#5618,.F.) ;
#7545 = ORIENTED_EDGE('',*,*,#5628,.F.) ;
#7546 = ORIENTED_EDGE('',*,*,#5629,.T.) ;
#7547 = ORIENTED_EDGE('',*,*,#5628,.T.) ;
#7548 = ORIENTED_EDGE('',*,*,#5617,.F.) ;
#7549 = ORIENTED_EDGE('',*,*,#5623,.F.) ;
#7550 = ORIENTED_EDGE('',*,*,#5612,.T.) ;
#7551 = ORIENTED_EDGE('',*,*,#5630,.F.) ;
#7552 = ORIENTED_EDGE('',*,*,#5620,.F.) ;
#7553 = ORIENTED_EDGE('',*,*,#5625,.F.) ;
#7554 = ORIENTED_EDGE('',*,*,#5631,.T.) ;
#7555 = ORIENTED_EDGE('',*,*,#5632,.F.) ;
#7556 = ORIENTED_EDGE('',*,*,#5631,.F.) ;
#7557 = ORIENTED_EDGE('',*,*,#5624,.F.) ;
#7558 = ORIENTED_EDGE('',*,*,#5627,.F.) ;
#7559 = ORIENTED_EDGE('',*,*,#5629,.F.) ;
#7560 = ORIENTED_EDGE('',*,*,#5622,.F.) ;
#7561 = ORIENTED_EDGE('',*,*,#5633,.F.) ;
#7562 = ORIENTED_EDGE('',*,*,#5634,.T.) ;
#7563 = ORIENTED_EDGE('',*,*,#5605,.T.) ;
#7564 = ORIENTED_EDGE('',*,*,#5635,.T.) ;
#7565 = ORIENTED_EDGE('',*,*,#5636,.T.) ;
#7566 = ORIENTED_EDGE('',*,*,#5637,.T.) ;
#7567 = ORIENTED_EDGE('',*,*,#5635,.F.) ;
#7568 = ORIENTED_EDGE('',*,*,#5606,.T.) ;
#7569 = ORIENTED_EDGE('',*,*,#5634,.F.) ;
#7570 = ORIENTED_EDGE('',*,*,#5602,.T.) ;
#7571 = ORIENTED_EDGE('',*,*,#5603,.T.) ;
#7572 = ORIENTED_EDGE('',*,*,#5636,.F.) ;
#7573 = ORIENTED_EDGE('',*,*,#5637,.F.) ;
#7574 = ORIENTED_EDGE('',*,*,#5638,.T.) ;
#7575 = ORIENTED_EDGE('',*,*,#5639,.T.) ;
#7576 = ORIENTED_EDGE('',*,*,#5640,.T.) ;
#7577 = ORIENTED_EDGE('',*,*,#5638,.F.) ;
#7578 = ORIENTED_EDGE('',*,*,#5640,.F.) ;
#7579 = ORIENTED_EDGE('',*,*,#5641,.T.) ;
#7580 = ORIENTED_EDGE('',*,*,#5642,.T.) ;
#7581 = ORIENTED_EDGE('',*,*,#5643,.T.) ;
#7582 = ORIENTED_EDGE('',*,*,#5641,.F.) ;
#7583 = ORIENTED_EDGE('',*,*,#5639,.F.) ;
#7584 = ORIENTED_EDGE('',*,*,#5642,.F.) ;
#7585 = ORIENTED_EDGE('',*,*,#5643,.F.) ;
#7586 = ORIENTED_EDGE('',*,*,#5644,.T.) ;
#7587 = ORIENTED_EDGE('',*,*,#5645,.T.) ;
#7588 = ORIENTED_EDGE('',*,*,#5646,.T.) ;
#7589 = ORIENTED_EDGE('',*,*,#5644,.F.) ;
#7590 = ORIENTED_EDGE('',*,*,#5646,.F.) ;
#7591 = ORIENTED_EDGE('',*,*,#5647,.T.) ;
#7592 = ORIENTED_EDGE('',*,*,#5610,.T.) ;
#7593 = ORIENTED_EDGE('',*,*,#5648,.T.) ;
#7594 = ORIENTED_EDGE('',*,*,#5649,.T.) ;
#7595 = ORIENTED_EDGE('',*,*,#5648,.F.) ;
#7596 = ORIENTED_EDGE('',*,*,#5609,.T.) ;
#7597 = ORIENTED_EDGE('',*,*,#5647,.F.) ;
#7598 = ORIENTED_EDGE('',*,*,#5645,.F.) ;
#7599 = ORIENTED_EDGE('',*,*,#5607,.T.) ;
#7600 = ORIENTED_EDGE('',*,*,#5611,.T.) ;
#7601 = ORIENTED_EDGE('',*,*,#5621,.T.) ;
#7602 = ORIENTED_EDGE('',*,*,#5615,.T.) ;
#7603 = ORIENTED_EDGE('',*,*,#5630,.T.) ;
#7604 = ORIENTED_EDGE('',*,*,#5632,.T.) ;
#7605 = ORIENTED_EDGE('',*,*,#5633,.T.) ;
#7606 = ORIENTED_EDGE('',*,*,#5649,.F.) ;
#7607 = ORIENTED_EDGE('',*,*,#5650,.F.) ;
#7608 = ORIENTED_EDGE('',*,*,#5651,.T.) ;
#7609 = ORIENTED_EDGE('',*,*,#5652,.T.) ;
#7610 = ORIENTED_EDGE('',*,*,#5651,.F.) ;
#7611 = ORIENTED_EDGE('',*,*,#5653,.T.) ;
#7612 = ORIENTED_EDGE('',*,*,#5654,.T.) ;
#7613 = ORIENTED_EDGE('',*,*,#5655,.F.) ;
#7614 = ORIENTED_EDGE('',*,*,#5656,.F.) ;
#7615 = ORIENTED_EDGE('',*,*,#5657,.T.) ;
#7616 = ORIENTED_EDGE('',*,*,#5656,.T.) ;
#7617 = ORIENTED_EDGE('',*,*,#5658,.F.) ;
#7618 = ORIENTED_EDGE('',*,*,#5659,.F.) ;
#7619 = ORIENTED_EDGE('',*,*,#5660,.T.) ;
#7620 = ORIENTED_EDGE('',*,*,#5659,.T.) ;
#7621 = ORIENTED_EDGE('',*,*,#5661,.F.) ;
#7622 = ORIENTED_EDGE('',*,*,#5662,.F.) ;
#7623 = ORIENTED_EDGE('',*,*,#5663,.T.) ;
#7624 = ORIENTED_EDGE('',*,*,#5662,.T.) ;
#7625 = ORIENTED_EDGE('',*,*,#5664,.F.) ;
#7626 = ORIENTED_EDGE('',*,*,#5654,.F.) ;
#7627 = ORIENTED_EDGE('',*,*,#5664,.T.) ;
#7628 = ORIENTED_EDGE('',*,*,#5661,.T.) ;
#7629 = ORIENTED_EDGE('',*,*,#5658,.T.) ;
#7630 = ORIENTED_EDGE('',*,*,#5655,.T.) ;
#7631 = ORIENTED_EDGE('',*,*,#5650,.T.) ;
#7632 = ORIENTED_EDGE('',*,*,#5663,.F.) ;
#7633 = ORIENTED_EDGE('',*,*,#5653,.F.) ;
#7634 = ORIENTED_EDGE('',*,*,#5657,.F.) ;
#7635 = ORIENTED_EDGE('',*,*,#5660,.F.) ;
#7636 = ORIENTED_EDGE('',*,*,#5652,.F.) ;
#7637 = ORIENTED_EDGE('',*,*,#5665,.F.) ;
#7638 = ORIENTED_EDGE('',*,*,#5666,.F.) ;
#7639 = ORIENTED_EDGE('',*,*,#5667,.T.) ;
#7640 = ORIENTED_EDGE('',*,*,#5665,.T.) ;
#7641 = ORIENTED_EDGE('',*,*,#5667,.F.) ;
#7642 = ORIENTED_EDGE('',*,*,#5668,.F.) ;
#7643 = ORIENTED_EDGE('',*,*,#5669,.T.) ;
#7644 = ORIENTED_EDGE('',*,*,#5666,.T.) ;
#7645 = ORIENTED_EDGE('',*,*,#5669,.F.) ;
#7646 = ORIENTED_EDGE('',*,*,#5668,.T.) ;
#7647 = ORIENTED_EDGE('',*,*,#5670,.F.) ;
#7648 = ORIENTED_EDGE('',*,*,#5671,.F.) ;
#7649 = ORIENTED_EDGE('',*,*,#5672,.T.) ;
#7650 = ORIENTED_EDGE('',*,*,#5670,.T.) ;
#7651 = ORIENTED_EDGE('',*,*,#5672,.F.) ;
#7652 = ORIENTED_EDGE('',*,*,#5671,.T.) ;
#7653 = ORIENTED_EDGE('',*,*,#5673,.F.) ;
#7654 = ORIENTED_EDGE('',*,*,#5674,.F.) ;
#7655 = ORIENTED_EDGE('',*,*,#5675,.T.) ;
#7656 = ORIENTED_EDGE('',*,*,#5673,.T.) ;
#7657 = ORIENTED_EDGE('',*,*,#5675,.F.) ;
#7658 = ORIENTED_EDGE('',*,*,#5676,.F.) ;
#7659 = ORIENTED_EDGE('',*,*,#5674,.T.) ;
#7660 = ORIENTED_EDGE('',*,*,#5677,.F.) ;
#7661 = ORIENTED_EDGE('',*,*,#5678,.T.) ;
#7662 = ORIENTED_EDGE('',*,*,#5676,.T.) ;
#7663 = ORIENTED_EDGE('',*,*,#5678,.F.) ;
#7664 = ORIENTED_EDGE('',*,*,#5679,.F.) ;
#7665 = ORIENTED_EDGE('',*,*,#5680,.T.) ;
#7666 = ORIENTED_EDGE('',*,*,#5677,.T.) ;
#7667 = ORIENTED_EDGE('',*,*,#5680,.F.) ;
#7668 = ORIENTED_EDGE('',*,*,#5679,.T.) ;
#7669 = ORIENTED_EDGE('',*,*,#5681,.F.) ;
#7670 = ORIENTED_EDGE('',*,*,#5682,.F.) ;
#7671 = ORIENTED_EDGE('',*,*,#5683,.F.) ;
#7672 = ORIENTED_EDGE('',*,*,#5684,.F.) ;
#7673 = ORIENTED_EDGE('',*,*,#5685,.F.) ;
#7674 = ORIENTED_EDGE('',*,*,#5686,.T.) ;
#7675 = ORIENTED_EDGE('',*,*,#5687,.F.) ;
#7676 = ORIENTED_EDGE('',*,*,#5688,.F.) ;
#7677 = ORIENTED_EDGE('',*,*,#5689,.F.) ;
#7678 = ORIENTED_EDGE('',*,*,#5684,.T.) ;
#7679 = ORIENTED_EDGE('',*,*,#5690,.F.) ;
#7680 = ORIENTED_EDGE('',*,*,#5691,.F.) ;
#7681 = ORIENTED_EDGE('',*,*,#5692,.F.) ;
#7682 = ORIENTED_EDGE('',*,*,#5693,.F.) ;
#7683 = ORIENTED_EDGE('',*,*,#5694,.F.) ;
#7684 = ORIENTED_EDGE('',*,*,#5686,.F.) ;
#7685 = ORIENTED_EDGE('',*,*,#5688,.T.) ;
#7686 = ORIENTED_EDGE('',*,*,#5695,.F.) ;
#7687 = ORIENTED_EDGE('',*,*,#5682,.T.) ;
#7688 = ORIENTED_EDGE('',*,*,#5696,.T.) ;
#7689 = ORIENTED_EDGE('',*,*,#5687,.T.) ;
#7690 = ORIENTED_EDGE('',*,*,#5694,.T.) ;
#7691 = ORIENTED_EDGE('',*,*,#5697,.F.) ;
#7692 = ORIENTED_EDGE('',*,*,#5690,.T.) ;
#7693 = ORIENTED_EDGE('',*,*,#5683,.T.) ;
#7694 = ORIENTED_EDGE('',*,*,#5695,.T.) ;
#7695 = ORIENTED_EDGE('',*,*,#5693,.T.) ;
#7696 = ORIENTED_EDGE('',*,*,#5698,.F.) ;
#7697 = ORIENTED_EDGE('',*,*,#5691,.T.) ;
#7698 = ORIENTED_EDGE('',*,*,#5697,.T.) ;
#7699 = ORIENTED_EDGE('',*,*,#5685,.T.) ;
#7700 = ORIENTED_EDGE('',*,*,#5696,.F.) ;
#7701 = ORIENTED_EDGE('',*,*,#5681,.T.) ;
#7702 = ORIENTED_EDGE('',*,*,#5689,.T.) ;
#7703 = ORIENTED_EDGE('',*,*,#5698,.T.) ;
#7704 = ORIENTED_EDGE('',*,*,#5692,.T.) ;
#7705 = ORIENTED_EDGE('',*,*,#5699,.F.) ;
#7706 = ORIENTED_EDGE('',*,*,#5700,.F.) ;
#7707 = ORIENTED_EDGE('',*,*,#5701,.T.) ;
#7708 = ORIENTED_EDGE('',*,*,#5699,.T.) ;
#7709 = ORIENTED_EDGE('',*,*,#5701,.F.) ;
#7710 = ORIENTED_EDGE('',*,*,#5702,.F.) ;
#7711 = ORIENTED_EDGE('',*,*,#5703,.T.) ;
#7712 = ORIENTED_EDGE('',*,*,#5700,.T.) ;
#7713 = ORIENTED_EDGE('',*,*,#5703,.F.) ;
#7714 = ORIENTED_EDGE('',*,*,#5704,.F.) ;
#7715 = ORIENTED_EDGE('',*,*,#5705,.T.) ;
#7716 = ORIENTED_EDGE('',*,*,#5702,.T.) ;
#7717 = ORIENTED_EDGE('',*,*,#5705,.F.) ;
#7718 = ORIENTED_EDGE('',*,*,#5704,.T.) ;
#7719 = ORIENTED_EDGE('',*,*,#5706,.F.) ;
#7720 = ORIENTED_EDGE('',*,*,#5707,.F.) ;
#7721 = ORIENTED_EDGE('',*,*,#5708,.T.) ;
#7722 = ORIENTED_EDGE('',*,*,#5706,.T.) ;
#7723 = ORIENTED_EDGE('',*,*,#5708,.F.) ;
#7724 = ORIENTED_EDGE('',*,*,#5709,.F.) ;
#7725 = ORIENTED_EDGE('',*,*,#5710,.T.) ;
#7726 = ORIENTED_EDGE('',*,*,#5707,.T.) ;
#7727 = ORIENTED_EDGE('',*,*,#5710,.F.) ;
#7728 = ORIENTED_EDGE('',*,*,#5709,.T.) ;
#7729 = ORIENTED_EDGE('',*,*,#5711,.F.) ;
#7730 = ORIENTED_EDGE('',*,*,#5712,.T.) ;
#7731 = ORIENTED_EDGE('',*,*,#5713,.F.) ;
#7732 = ORIENTED_EDGE('',*,*,#5714,.T.) ;
#7733 = ORIENTED_EDGE('',*,*,#5715,.F.) ;
#7734 = ORIENTED_EDGE('',*,*,#5716,.T.) ;
#7735 = ORIENTED_EDGE('',*,*,#5711,.T.) ;
#7736 = ORIENTED_EDGE('',*,*,#5717,.T.) ;
#7737 = ORIENTED_EDGE('',*,*,#5718,.F.) ;
#7738 = ORIENTED_EDGE('',*,*,#5719,.T.) ;
#7739 = ORIENTED_EDGE('',*,*,#5715,.T.) ;
#7740 = ORIENTED_EDGE('',*,*,#5720,.T.) ;
#7741 = ORIENTED_EDGE('',*,*,#5721,.F.) ;
#7742 = ORIENTED_EDGE('',*,*,#5722,.T.) ;
#7743 = ORIENTED_EDGE('',*,*,#5718,.T.) ;
#7744 = ORIENTED_EDGE('',*,*,#5723,.T.) ;
#7745 = ORIENTED_EDGE('',*,*,#5724,.F.) ;
#7746 = ORIENTED_EDGE('',*,*,#5725,.T.) ;
#7747 = ORIENTED_EDGE('',*,*,#5721,.T.) ;
#7748 = ORIENTED_EDGE('',*,*,#5726,.T.) ;
#7749 = ORIENTED_EDGE('',*,*,#5727,.F.) ;
#7750 = ORIENTED_EDGE('',*,*,#5728,.T.) ;
#7751 = ORIENTED_EDGE('',*,*,#5724,.T.) ;
#7752 = ORIENTED_EDGE('',*,*,#5729,.T.) ;
#7753 = ORIENTED_EDGE('',*,*,#5730,.F.) ;
#7754 = ORIENTED_EDGE('',*,*,#5731,.T.) ;
#7755 = ORIENTED_EDGE('',*,*,#5727,.T.) ;
#7756 = ORIENTED_EDGE('',*,*,#5732,.T.) ;
#7757 = ORIENTED_EDGE('',*,*,#5733,.F.) ;
#7758 = ORIENTED_EDGE('',*,*,#5734,.T.) ;
#7759 = ORIENTED_EDGE('',*,*,#5730,.T.) ;
#7760 = ORIENTED_EDGE('',*,*,#5735,.T.) ;
#7761 = ORIENTED_EDGE('',*,*,#5736,.F.) ;
#7762 = ORIENTED_EDGE('',*,*,#5737,.T.) ;
#7763 = ORIENTED_EDGE('',*,*,#5733,.T.) ;
#7764 = ORIENTED_EDGE('',*,*,#5738,.T.) ;
#7765 = ORIENTED_EDGE('',*,*,#5739,.F.) ;
#7766 = ORIENTED_EDGE('',*,*,#5740,.T.) ;
#7767 = ORIENTED_EDGE('',*,*,#5736,.T.) ;
#7768 = ORIENTED_EDGE('',*,*,#5741,.T.) ;
#7769 = ORIENTED_EDGE('',*,*,#5742,.F.) ;
#7770 = ORIENTED_EDGE('',*,*,#5743,.T.) ;
#7771 = ORIENTED_EDGE('',*,*,#5739,.T.) ;
#7772 = ORIENTED_EDGE('',*,*,#5744,.T.) ;
#7773 = ORIENTED_EDGE('',*,*,#5745,.F.) ;
#7774 = ORIENTED_EDGE('',*,*,#5746,.T.) ;
#7775 = ORIENTED_EDGE('',*,*,#5742,.T.) ;
#7776 = ORIENTED_EDGE('',*,*,#5747,.T.) ;
#7777 = ORIENTED_EDGE('',*,*,#5748,.F.) ;
#7778 = ORIENTED_EDGE('',*,*,#5749,.T.) ;
#7779 = ORIENTED_EDGE('',*,*,#5745,.T.) ;
#7780 = ORIENTED_EDGE('',*,*,#5750,.T.) ;
#7781 = ORIENTED_EDGE('',*,*,#5751,.F.) ;
#7782 = ORIENTED_EDGE('',*,*,#5752,.T.) ;
#7783 = ORIENTED_EDGE('',*,*,#5748,.T.) ;
#7784 = ORIENTED_EDGE('',*,*,#5753,.T.) ;
#7785 = ORIENTED_EDGE('',*,*,#5754,.F.) ;
#7786 = ORIENTED_EDGE('',*,*,#5755,.T.) ;
#7787 = ORIENTED_EDGE('',*,*,#5756,.F.) ;
#7788 = ORIENTED_EDGE('',*,*,#5757,.F.) ;
#7789 = ORIENTED_EDGE('',*,*,#5758,.F.) ;
#7790 = ORIENTED_EDGE('',*,*,#5759,.T.) ;
#7791 = ORIENTED_EDGE('',*,*,#5754,.T.) ;
#7792 = ORIENTED_EDGE('',*,*,#5760,.F.) ;
#7793 = ORIENTED_EDGE('',*,*,#5761,.F.) ;
#7794 = ORIENTED_EDGE('',*,*,#5762,.T.) ;
#7795 = ORIENTED_EDGE('',*,*,#5758,.T.) ;
#7796 = ORIENTED_EDGE('',*,*,#5763,.F.) ;
#7797 = ORIENTED_EDGE('',*,*,#5764,.F.) ;
#7798 = ORIENTED_EDGE('',*,*,#5765,.T.) ;
#7799 = ORIENTED_EDGE('',*,*,#5761,.T.) ;
#7800 = ORIENTED_EDGE('',*,*,#5766,.F.) ;
#7801 = ORIENTED_EDGE('',*,*,#5767,.F.) ;
#7802 = ORIENTED_EDGE('',*,*,#5768,.T.) ;
#7803 = ORIENTED_EDGE('',*,*,#5764,.T.) ;
#7804 = ORIENTED_EDGE('',*,*,#5769,.F.) ;
#7805 = ORIENTED_EDGE('',*,*,#5770,.F.) ;
#7806 = ORIENTED_EDGE('',*,*,#5771,.T.) ;
#7807 = ORIENTED_EDGE('',*,*,#5767,.T.) ;
#7808 = ORIENTED_EDGE('',*,*,#5772,.F.) ;
#7809 = ORIENTED_EDGE('',*,*,#5773,.F.) ;
#7810 = ORIENTED_EDGE('',*,*,#5774,.T.) ;
#7811 = ORIENTED_EDGE('',*,*,#5770,.T.) ;
#7812 = ORIENTED_EDGE('',*,*,#5775,.F.) ;
#7813 = ORIENTED_EDGE('',*,*,#5776,.F.) ;
#7814 = ORIENTED_EDGE('',*,*,#5777,.T.) ;
#7815 = ORIENTED_EDGE('',*,*,#5773,.T.) ;
#7816 = ORIENTED_EDGE('',*,*,#5778,.F.) ;
#7817 = ORIENTED_EDGE('',*,*,#5779,.F.) ;
#7818 = ORIENTED_EDGE('',*,*,#5780,.T.) ;
#7819 = ORIENTED_EDGE('',*,*,#5776,.T.) ;
#7820 = ORIENTED_EDGE('',*,*,#5781,.F.) ;
#7821 = ORIENTED_EDGE('',*,*,#5782,.F.) ;
#7822 = ORIENTED_EDGE('',*,*,#5783,.T.) ;
#7823 = ORIENTED_EDGE('',*,*,#5779,.T.) ;
#7824 = ORIENTED_EDGE('',*,*,#5784,.F.) ;
#7825 = ORIENTED_EDGE('',*,*,#5785,.F.) ;
#7826 = ORIENTED_EDGE('',*,*,#5786,.T.) ;
#7827 = ORIENTED_EDGE('',*,*,#5782,.T.) ;
#7828 = ORIENTED_EDGE('',*,*,#5787,.F.) ;
#7829 = ORIENTED_EDGE('',*,*,#5788,.F.) ;
#7830 = ORIENTED_EDGE('',*,*,#5789,.T.) ;
#7831 = ORIENTED_EDGE('',*,*,#5785,.T.) ;
#7832 = ORIENTED_EDGE('',*,*,#5790,.F.) ;
#7833 = ORIENTED_EDGE('',*,*,#5791,.F.) ;
#7834 = ORIENTED_EDGE('',*,*,#5792,.T.) ;
#7835 = ORIENTED_EDGE('',*,*,#5788,.T.) ;
#7836 = ORIENTED_EDGE('',*,*,#5793,.F.) ;
#7837 = ORIENTED_EDGE('',*,*,#5794,.F.) ;
#7838 = ORIENTED_EDGE('',*,*,#5795,.T.) ;
#7839 = ORIENTED_EDGE('',*,*,#5791,.T.) ;
#7840 = ORIENTED_EDGE('',*,*,#5796,.F.) ;
#7841 = ORIENTED_EDGE('',*,*,#5756,.T.) ;
#7842 = ORIENTED_EDGE('',*,*,#5797,.T.) ;
#7843 = ORIENTED_EDGE('',*,*,#5798,.F.) ;
#7844 = ORIENTED_EDGE('',*,*,#5799,.F.) ;
#7845 = ORIENTED_EDGE('',*,*,#5800,.T.) ;
#7846 = ORIENTED_EDGE('',*,*,#5800,.F.) ;
#7847 = ORIENTED_EDGE('',*,*,#5801,.F.) ;
#7848 = ORIENTED_EDGE('',*,*,#5753,.F.) ;
#7849 = ORIENTED_EDGE('',*,*,#5750,.F.) ;
#7850 = ORIENTED_EDGE('',*,*,#5747,.F.) ;
#7851 = ORIENTED_EDGE('',*,*,#5744,.F.) ;
#7852 = ORIENTED_EDGE('',*,*,#5741,.F.) ;
#7853 = ORIENTED_EDGE('',*,*,#5738,.F.) ;
#7854 = ORIENTED_EDGE('',*,*,#5735,.F.) ;
#7855 = ORIENTED_EDGE('',*,*,#5732,.F.) ;
#7856 = ORIENTED_EDGE('',*,*,#5729,.F.) ;
#7857 = ORIENTED_EDGE('',*,*,#5726,.F.) ;
#7858 = ORIENTED_EDGE('',*,*,#5723,.F.) ;
#7859 = ORIENTED_EDGE('',*,*,#5720,.F.) ;
#7860 = ORIENTED_EDGE('',*,*,#5717,.F.) ;
#7861 = ORIENTED_EDGE('',*,*,#5714,.F.) ;
#7862 = ORIENTED_EDGE('',*,*,#5802,.F.) ;
#7863 = ORIENTED_EDGE('',*,*,#5803,.T.) ;
#7864 = ORIENTED_EDGE('',*,*,#5796,.T.) ;
#7865 = ORIENTED_EDGE('',*,*,#5793,.T.) ;
#7866 = ORIENTED_EDGE('',*,*,#5790,.T.) ;
#7867 = ORIENTED_EDGE('',*,*,#5787,.T.) ;
#7868 = ORIENTED_EDGE('',*,*,#5784,.T.) ;
#7869 = ORIENTED_EDGE('',*,*,#5781,.T.) ;
#7870 = ORIENTED_EDGE('',*,*,#5778,.T.) ;
#7871 = ORIENTED_EDGE('',*,*,#5775,.T.) ;
#7872 = ORIENTED_EDGE('',*,*,#5772,.T.) ;
#7873 = ORIENTED_EDGE('',*,*,#5769,.T.) ;
#7874 = ORIENTED_EDGE('',*,*,#5766,.T.) ;
#7875 = ORIENTED_EDGE('',*,*,#5763,.T.) ;
#7876 = ORIENTED_EDGE('',*,*,#5760,.T.) ;
#7877 = ORIENTED_EDGE('',*,*,#5757,.T.) ;
#7878 = ORIENTED_EDGE('',*,*,#5804,.F.) ;
#7879 = ORIENTED_EDGE('',*,*,#5805,.T.) ;
#7880 = ORIENTED_EDGE('',*,*,#5806,.T.) ;
#7881 = ORIENTED_EDGE('',*,*,#5802,.T.) ;
#7882 = ORIENTED_EDGE('',*,*,#5807,.F.) ;
#7883 = ORIENTED_EDGE('',*,*,#5794,.T.) ;
#7884 = ORIENTED_EDGE('',*,*,#5803,.F.) ;
#7885 = ORIENTED_EDGE('',*,*,#5806,.F.) ;
#7886 = ORIENTED_EDGE('',*,*,#5808,.T.) ;
#7887 = ORIENTED_EDGE('',*,*,#5797,.F.) ;
#7888 = ORIENTED_EDGE('',*,*,#5755,.F.) ;
#7889 = ORIENTED_EDGE('',*,*,#5759,.F.) ;
#7890 = ORIENTED_EDGE('',*,*,#5762,.F.) ;
#7891 = ORIENTED_EDGE('',*,*,#5765,.F.) ;
#7892 = ORIENTED_EDGE('',*,*,#5768,.F.) ;
#7893 = ORIENTED_EDGE('',*,*,#5771,.F.) ;
#7894 = ORIENTED_EDGE('',*,*,#5774,.F.) ;
#7895 = ORIENTED_EDGE('',*,*,#5777,.F.) ;
#7896 = ORIENTED_EDGE('',*,*,#5780,.F.) ;
#7897 = ORIENTED_EDGE('',*,*,#5783,.F.) ;
#7898 = ORIENTED_EDGE('',*,*,#5786,.F.) ;
#7899 = ORIENTED_EDGE('',*,*,#5789,.F.) ;
#7900 = ORIENTED_EDGE('',*,*,#5792,.F.) ;
#7901 = ORIENTED_EDGE('',*,*,#5795,.F.) ;
#7902 = ORIENTED_EDGE('',*,*,#5808,.F.) ;
#7903 = ORIENTED_EDGE('',*,*,#5805,.F.) ;
#7904 = ORIENTED_EDGE('',*,*,#5712,.F.) ;
#7905 = ORIENTED_EDGE('',*,*,#5716,.F.) ;
#7906 = ORIENTED_EDGE('',*,*,#5719,.F.) ;
#7907 = ORIENTED_EDGE('',*,*,#5722,.F.) ;
#7908 = ORIENTED_EDGE('',*,*,#5725,.F.) ;
#7909 = ORIENTED_EDGE('',*,*,#5728,.F.) ;
#7910 = ORIENTED_EDGE('',*,*,#5731,.F.) ;
#7911 = ORIENTED_EDGE('',*,*,#5734,.F.) ;
#7912 = ORIENTED_EDGE('',*,*,#5737,.F.) ;
#7913 = ORIENTED_EDGE('',*,*,#5740,.F.) ;
#7914 = ORIENTED_EDGE('',*,*,#5743,.F.) ;
#7915 = ORIENTED_EDGE('',*,*,#5746,.F.) ;
#7916 = ORIENTED_EDGE('',*,*,#5749,.F.) ;
#7917 = ORIENTED_EDGE('',*,*,#5752,.F.) ;
#7918 = ORIENTED_EDGE('',*,*,#5809,.F.) ;
#7919 = ORIENTED_EDGE('',*,*,#5804,.T.) ;
#7920 = ORIENTED_EDGE('',*,*,#5810,.T.) ;
#7921 = ORIENTED_EDGE('',*,*,#5811,.T.) ;
#7922 = ORIENTED_EDGE('',*,*,#5810,.F.) ;
#7923 = ORIENTED_EDGE('',*,*,#5807,.T.) ;
#7924 = ORIENTED_EDGE('',*,*,#5713,.T.) ;
#7925 = ORIENTED_EDGE('',*,*,#5751,.T.) ;
#7926 = ORIENTED_EDGE('',*,*,#5801,.T.) ;
#7927 = ORIENTED_EDGE('',*,*,#5812,.F.) ;
#7928 = ORIENTED_EDGE('',*,*,#5809,.T.) ;
#7929 = ORIENTED_EDGE('',*,*,#5813,.F.) ;
#7930 = ORIENTED_EDGE('',*,*,#5811,.F.) ;
#7931 = ORIENTED_EDGE('',*,*,#5799,.T.) ;
#7932 = ORIENTED_EDGE('',*,*,#5814,.T.) ;
#7933 = ORIENTED_EDGE('',*,*,#5815,.T.) ;
#7934 = ORIENTED_EDGE('',*,*,#5814,.F.) ;
#7935 = ORIENTED_EDGE('',*,*,#5798,.T.) ;
#7936 = ORIENTED_EDGE('',*,*,#5812,.T.) ;
#7937 = ORIENTED_EDGE('',*,*,#5815,.F.) ;
#7938 = ORIENTED_EDGE('',*,*,#5816,.F.) ;
#7939 = ORIENTED_EDGE('',*,*,#5817,.F.) ;
#7940 = ORIENTED_EDGE('',*,*,#5818,.F.) ;
#7941 = ORIENTED_EDGE('',*,*,#5819,.F.) ;
#7942 = ORIENTED_EDGE('',*,*,#5818,.T.) ;
#7943 = ORIENTED_EDGE('',*,*,#5820,.F.) ;
#7944 = ORIENTED_EDGE('',*,*,#5821,.F.) ;
#7945 = ORIENTED_EDGE('',*,*,#5822,.F.) ;
#7946 = ORIENTED_EDGE('',*,*,#5823,.F.) ;
#7947 = ORIENTED_EDGE('',*,*,#5820,.T.) ;
#7948 = ORIENTED_EDGE('',*,*,#5817,.T.) ;
#7949 = ORIENTED_EDGE('',*,*,#5822,.T.) ;
#7950 = ORIENTED_EDGE('',*,*,#5816,.T.) ;
#7951 = ORIENTED_EDGE('',*,*,#5819,.T.) ;
#7952 = ORIENTED_EDGE('',*,*,#5824,.F.) ;
#7953 = ORIENTED_EDGE('',*,*,#5825,.T.) ;
#7954 = ORIENTED_EDGE('',*,*,#5826,.T.) ;
#7955 = ORIENTED_EDGE('',*,*,#5827,.T.) ;
#7956 = ORIENTED_EDGE('',*,*,#5828,.F.) ;
#7957 = ORIENTED_EDGE('',*,*,#5829,.T.) ;
#7958 = ORIENTED_EDGE('',*,*,#5830,.T.) ;
#7959 = ORIENTED_EDGE('',*,*,#5831,.T.) ;
#7960 = ORIENTED_EDGE('',*,*,#5832,.F.) ;
#7961 = ORIENTED_EDGE('',*,*,#5833,.T.) ;
#7962 = ORIENTED_EDGE('',*,*,#5834,.T.) ;
#7963 = ORIENTED_EDGE('',*,*,#5835,.T.) ;
#7964 = ORIENTED_EDGE('',*,*,#5836,.F.) ;
#7965 = ORIENTED_EDGE('',*,*,#5837,.T.) ;
#7966 = ORIENTED_EDGE('',*,*,#5838,.T.) ;
#7967 = ORIENTED_EDGE('',*,*,#5839,.T.) ;
#7968 = ORIENTED_EDGE('',*,*,#5840,.F.) ;
#7969 = ORIENTED_EDGE('',*,*,#5841,.T.) ;
#7970 = ORIENTED_EDGE('',*,*,#5842,.T.) ;
#7971 = ORIENTED_EDGE('',*,*,#5843,.T.) ;
#7972 = ORIENTED_EDGE('',*,*,#5844,.F.) ;
#7973 = ORIENTED_EDGE('',*,*,#5845,.T.) ;
#7974 = ORIENTED_EDGE('',*,*,#5846,.T.) ;
#7975 = ORIENTED_EDGE('',*,*,#5847,.T.) ;
#7976 = ORIENTED_EDGE('',*,*,#5848,.F.) ;
#7977 = ORIENTED_EDGE('',*,*,#5849,.T.) ;
#7978 = ORIENTED_EDGE('',*,*,#5850,.T.) ;
#7979 = ORIENTED_EDGE('',*,*,#5851,.T.) ;
#7980 = ORIENTED_EDGE('',*,*,#5852,.F.) ;
#7981 = ORIENTED_EDGE('',*,*,#5853,.T.) ;
#7982 = ORIENTED_EDGE('',*,*,#5854,.T.) ;
#7983 = ORIENTED_EDGE('',*,*,#5855,.T.) ;
#7984 = ORIENTED_EDGE('',*,*,#5856,.F.) ;
#7985 = ORIENTED_EDGE('',*,*,#5857,.T.) ;
#7986 = ORIENTED_EDGE('',*,*,#5858,.T.) ;
#7987 = ORIENTED_EDGE('',*,*,#5859,.T.) ;
#7988 = ORIENTED_EDGE('',*,*,#5860,.F.) ;
#7989 = ORIENTED_EDGE('',*,*,#5861,.T.) ;
#7990 = ORIENTED_EDGE('',*,*,#5862,.T.) ;
#7991 = ORIENTED_EDGE('',*,*,#5863,.T.) ;
#7992 = ORIENTED_EDGE('',*,*,#5864,.F.) ;
#7993 = ORIENTED_EDGE('',*,*,#5865,.T.) ;
#7994 = ORIENTED_EDGE('',*,*,#5866,.T.) ;
#7995 = ORIENTED_EDGE('',*,*,#5867,.T.) ;
#7996 = ORIENTED_EDGE('',*,*,#5868,.F.) ;
#7997 = ORIENTED_EDGE('',*,*,#5869,.T.) ;
#7998 = ORIENTED_EDGE('',*,*,#5870,.T.) ;
#7999 = ORIENTED_EDGE('',*,*,#5871,.T.) ;
#8000 = ORIENTED_EDGE('',*,*,#5872,.F.) ;
#8001 = ORIENTED_EDGE('',*,*,#5873,.T.) ;
#8002 = ORIENTED_EDGE('',*,*,#5874,.T.) ;
#8003 = ORIENTED_EDGE('',*,*,#5875,.T.) ;
#8004 = ORIENTED_EDGE('',*,*,#5876,.F.) ;
#8005 = ORIENTED_EDGE('',*,*,#5877,.T.) ;
#8006 = ORIENTED_EDGE('',*,*,#5878,.T.) ;
#8007 = ORIENTED_EDGE('',*,*,#5879,.T.) ;
#8008 = ORIENTED_EDGE('',*,*,#5880,.F.) ;
#8009 = ORIENTED_EDGE('',*,*,#5881,.T.) ;
#8010 = ORIENTED_EDGE('',*,*,#5882,.T.) ;
#8011 = ORIENTED_EDGE('',*,*,#5883,.T.) ;
#8012 = ORIENTED_EDGE('',*,*,#5884,.F.) ;
#8013 = ORIENTED_EDGE('',*,*,#5885,.T.) ;
#8014 = ORIENTED_EDGE('',*,*,#5886,.T.) ;
#8015 = ORIENTED_EDGE('',*,*,#5887,.T.) ;
#8016 = ORIENTED_EDGE('',*,*,#5888,.F.) ;
#8017 = ORIENTED_EDGE('',*,*,#5889,.T.) ;
#8018 = ORIENTED_EDGE('',*,*,#5890,.T.) ;
#8019 = ORIENTED_EDGE('',*,*,#5891,.T.) ;
#8020 = ORIENTED_EDGE('',*,*,#5892,.F.) ;
#8021 = ORIENTED_EDGE('',*,*,#5893,.T.) ;
#8022 = ORIENTED_EDGE('',*,*,#5894,.T.) ;
#8023 = ORIENTED_EDGE('',*,*,#5895,.T.) ;
#8024 = ORIENTED_EDGE('',*,*,#5896,.F.) ;
#8025 = ORIENTED_EDGE('',*,*,#5897,.T.) ;
#8026 = ORIENTED_EDGE('',*,*,#5898,.T.) ;
#8027 = ORIENTED_EDGE('',*,*,#5899,.T.) ;
#8028 = ORIENTED_EDGE('',*,*,#5900,.F.) ;
#8029 = ORIENTED_EDGE('',*,*,#5899,.F.) ;
#8030 = ORIENTED_EDGE('',*,*,#5901,.T.) ;
#8031 = ORIENTED_EDGE('',*,*,#5902,.T.) ;
#8032 = ORIENTED_EDGE('',*,*,#5903,.F.) ;
#8033 = ORIENTED_EDGE('',*,*,#5904,.T.) ;
#8034 = ORIENTED_EDGE('',*,*,#5905,.T.) ;
#8035 = ORIENTED_EDGE('',*,*,#5906,.T.) ;
#8036 = ORIENTED_EDGE('',*,*,#5907,.F.) ;
#8037 = ORIENTED_EDGE('',*,*,#5908,.T.) ;
#8038 = ORIENTED_EDGE('',*,*,#5909,.T.) ;
#8039 = ORIENTED_EDGE('',*,*,#5910,.T.) ;
#8040 = ORIENTED_EDGE('',*,*,#5911,.F.) ;
#8041 = ORIENTED_EDGE('',*,*,#5912,.T.) ;
#8042 = ORIENTED_EDGE('',*,*,#5913,.T.) ;
#8043 = ORIENTED_EDGE('',*,*,#5914,.T.) ;
#8044 = ORIENTED_EDGE('',*,*,#5915,.F.) ;
#8045 = ORIENTED_EDGE('',*,*,#5916,.T.) ;
#8046 = ORIENTED_EDGE('',*,*,#5917,.T.) ;
#8047 = ORIENTED_EDGE('',*,*,#5918,.T.) ;
#8048 = ORIENTED_EDGE('',*,*,#5919,.F.) ;
#8049 = ORIENTED_EDGE('',*,*,#5920,.T.) ;
#8050 = ORIENTED_EDGE('',*,*,#5921,.T.) ;
#8051 = ORIENTED_EDGE('',*,*,#5922,.T.) ;
#8052 = ORIENTED_EDGE('',*,*,#5923,.F.) ;
#8053 = ORIENTED_EDGE('',*,*,#5924,.T.) ;
#8054 = ORIENTED_EDGE('',*,*,#5925,.T.) ;
#8055 = ORIENTED_EDGE('',*,*,#5926,.T.) ;
#8056 = ORIENTED_EDGE('',*,*,#5927,.F.) ;
#8057 = ORIENTED_EDGE('',*,*,#5928,.T.) ;
#8058 = ORIENTED_EDGE('',*,*,#5929,.T.) ;
#8059 = ORIENTED_EDGE('',*,*,#5930,.T.) ;
#8060 = ORIENTED_EDGE('',*,*,#5931,.F.) ;
#8061 = ORIENTED_EDGE('',*,*,#5932,.T.) ;
#8062 = ORIENTED_EDGE('',*,*,#5933,.T.) ;
#8063 = ORIENTED_EDGE('',*,*,#5934,.T.) ;
#8064 = ORIENTED_EDGE('',*,*,#5935,.F.) ;
#8065 = ORIENTED_EDGE('',*,*,#5936,.T.) ;
#8066 = ORIENTED_EDGE('',*,*,#5937,.T.) ;
#8067 = ORIENTED_EDGE('',*,*,#5938,.T.) ;
#8068 = ORIENTED_EDGE('',*,*,#5939,.F.) ;
#8069 = ORIENTED_EDGE('',*,*,#5940,.T.) ;
#8070 = ORIENTED_EDGE('',*,*,#5941,.T.) ;
#8071 = ORIENTED_EDGE('',*,*,#5942,.T.) ;
#8072 = ORIENTED_EDGE('',*,*,#5943,.F.) ;
#8073 = ORIENTED_EDGE('',*,*,#5944,.T.) ;
#8074 = ORIENTED_EDGE('',*,*,#5945,.T.) ;
#8075 = ORIENTED_EDGE('',*,*,#5946,.T.) ;
#8076 = ORIENTED_EDGE('',*,*,#5947,.F.) ;
#8077 = ORIENTED_EDGE('',*,*,#5948,.T.) ;
#8078 = ORIENTED_EDGE('',*,*,#5949,.T.) ;
#8079 = ORIENTED_EDGE('',*,*,#5950,.T.) ;
#8080 = ORIENTED_EDGE('',*,*,#5951,.F.) ;
#8081 = ORIENTED_EDGE('',*,*,#5952,.T.) ;
#8082 = ORIENTED_EDGE('',*,*,#5953,.T.) ;
#8083 = ORIENTED_EDGE('',*,*,#5954,.T.) ;
#8084 = ORIENTED_EDGE('',*,*,#5955,.F.) ;
#8085 = ORIENTED_EDGE('',*,*,#5956,.T.) ;
#8086 = ORIENTED_EDGE('',*,*,#5957,.T.) ;
#8087 = ORIENTED_EDGE('',*,*,#5958,.T.) ;
#8088 = ORIENTED_EDGE('',*,*,#5959,.F.) ;
#8089 = ORIENTED_EDGE('',*,*,#5960,.T.) ;
#8090 = ORIENTED_EDGE('',*,*,#5961,.T.) ;
#8091 = ORIENTED_EDGE('',*,*,#5962,.T.) ;
#8092 = ORIENTED_EDGE('',*,*,#5963,.F.) ;
#8093 = ORIENTED_EDGE('',*,*,#5964,.T.) ;
#8094 = ORIENTED_EDGE('',*,*,#5965,.T.) ;
#8095 = ORIENTED_EDGE('',*,*,#5966,.T.) ;
#8096 = ORIENTED_EDGE('',*,*,#5967,.F.) ;
#8097 = ORIENTED_EDGE('',*,*,#5966,.F.) ;
#8098 = ORIENTED_EDGE('',*,*,#5968,.T.) ;
#8099 = ORIENTED_EDGE('',*,*,#5969,.F.) ;
#8100 = ORIENTED_EDGE('',*,*,#5970,.F.) ;
#8101 = ORIENTED_EDGE('',*,*,#5971,.F.) ;
#8102 = ORIENTED_EDGE('',*,*,#5969,.T.) ;
#8103 = ORIENTED_EDGE('',*,*,#5972,.T.) ;
#8104 = ORIENTED_EDGE('',*,*,#5964,.F.) ;
#8105 = ORIENTED_EDGE('',*,*,#5965,.F.) ;
#8106 = ORIENTED_EDGE('',*,*,#5972,.F.) ;
#8107 = ORIENTED_EDGE('',*,*,#5968,.F.) ;
#8108 = ORIENTED_EDGE('',*,*,#5973,.T.) ;
#8109 = ORIENTED_EDGE('',*,*,#5974,.T.) ;
#8110 = ORIENTED_EDGE('',*,*,#5975,.T.) ;
#8111 = ORIENTED_EDGE('',*,*,#5896,.T.) ;
#8112 = ORIENTED_EDGE('',*,*,#5976,.T.) ;
#8113 = ORIENTED_EDGE('',*,*,#5977,.T.) ;
#8114 = ORIENTED_EDGE('',*,*,#5892,.T.) ;
#8115 = ORIENTED_EDGE('',*,*,#5978,.T.) ;
#8116 = ORIENTED_EDGE('',*,*,#5979,.T.) ;
#8117 = ORIENTED_EDGE('',*,*,#5888,.T.) ;
#8118 = ORIENTED_EDGE('',*,*,#5980,.T.) ;
#8119 = ORIENTED_EDGE('',*,*,#5981,.T.) ;
#8120 = ORIENTED_EDGE('',*,*,#5884,.T.) ;
#8121 = ORIENTED_EDGE('',*,*,#5982,.T.) ;
#8122 = ORIENTED_EDGE('',*,*,#5983,.T.) ;
#8123 = ORIENTED_EDGE('',*,*,#5880,.T.) ;
#8124 = ORIENTED_EDGE('',*,*,#5984,.T.) ;
#8125 = ORIENTED_EDGE('',*,*,#5985,.T.) ;
#8126 = ORIENTED_EDGE('',*,*,#5876,.T.) ;
#8127 = ORIENTED_EDGE('',*,*,#5986,.T.) ;
#8128 = ORIENTED_EDGE('',*,*,#5987,.T.) ;
#8129 = ORIENTED_EDGE('',*,*,#5872,.T.) ;
#8130 = ORIENTED_EDGE('',*,*,#5988,.T.) ;
#8131 = ORIENTED_EDGE('',*,*,#5989,.T.) ;
#8132 = ORIENTED_EDGE('',*,*,#5868,.T.) ;
#8133 = ORIENTED_EDGE('',*,*,#5990,.T.) ;
#8134 = ORIENTED_EDGE('',*,*,#5991,.T.) ;
#8135 = ORIENTED_EDGE('',*,*,#5864,.T.) ;
#8136 = ORIENTED_EDGE('',*,*,#5992,.T.) ;
#8137 = ORIENTED_EDGE('',*,*,#5993,.T.) ;
#8138 = ORIENTED_EDGE('',*,*,#5860,.T.) ;
#8139 = ORIENTED_EDGE('',*,*,#5994,.T.) ;
#8140 = ORIENTED_EDGE('',*,*,#5995,.T.) ;
#8141 = ORIENTED_EDGE('',*,*,#5856,.T.) ;
#8142 = ORIENTED_EDGE('',*,*,#5996,.T.) ;
#8143 = ORIENTED_EDGE('',*,*,#5997,.T.) ;
#8144 = ORIENTED_EDGE('',*,*,#5852,.T.) ;
#8145 = ORIENTED_EDGE('',*,*,#5998,.T.) ;
#8146 = ORIENTED_EDGE('',*,*,#5999,.T.) ;
#8147 = ORIENTED_EDGE('',*,*,#5848,.T.) ;
#8148 = ORIENTED_EDGE('',*,*,#6000,.T.) ;
#8149 = ORIENTED_EDGE('',*,*,#6001,.T.) ;
#8150 = ORIENTED_EDGE('',*,*,#5844,.T.) ;
#8151 = ORIENTED_EDGE('',*,*,#6002,.T.) ;
#8152 = ORIENTED_EDGE('',*,*,#6003,.T.) ;
#8153 = ORIENTED_EDGE('',*,*,#5840,.T.) ;
#8154 = ORIENTED_EDGE('',*,*,#6004,.T.) ;
#8155 = ORIENTED_EDGE('',*,*,#6005,.T.) ;
#8156 = ORIENTED_EDGE('',*,*,#5836,.T.) ;
#8157 = ORIENTED_EDGE('',*,*,#6006,.T.) ;
#8158 = ORIENTED_EDGE('',*,*,#6007,.T.) ;
#8159 = ORIENTED_EDGE('',*,*,#5832,.T.) ;
#8160 = ORIENTED_EDGE('',*,*,#6008,.T.) ;
#8161 = ORIENTED_EDGE('',*,*,#6009,.T.) ;
#8162 = ORIENTED_EDGE('',*,*,#5828,.T.) ;
#8163 = ORIENTED_EDGE('',*,*,#6010,.T.) ;
#8164 = ORIENTED_EDGE('',*,*,#6011,.T.) ;
#8165 = ORIENTED_EDGE('',*,*,#5824,.T.) ;
#8166 = ORIENTED_EDGE('',*,*,#5821,.T.) ;
#8167 = ORIENTED_EDGE('',*,*,#5823,.T.) ;
#8168 = ORIENTED_EDGE('',*,*,#5967,.T.) ;
#8169 = ORIENTED_EDGE('',*,*,#5970,.T.) ;
#8170 = ORIENTED_EDGE('',*,*,#5971,.T.) ;
#8171 = ORIENTED_EDGE('',*,*,#5963,.T.) ;
#8172 = ORIENTED_EDGE('',*,*,#6012,.T.) ;
#8173 = ORIENTED_EDGE('',*,*,#6013,.T.) ;
#8174 = ORIENTED_EDGE('',*,*,#5959,.T.) ;
#8175 = ORIENTED_EDGE('',*,*,#6014,.T.) ;
#8176 = ORIENTED_EDGE('',*,*,#6015,.T.) ;
#8177 = ORIENTED_EDGE('',*,*,#5955,.T.) ;
#8178 = ORIENTED_EDGE('',*,*,#6016,.T.) ;
#8179 = ORIENTED_EDGE('',*,*,#6017,.T.) ;
#8180 = ORIENTED_EDGE('',*,*,#5951,.T.) ;
#8181 = ORIENTED_EDGE('',*,*,#6018,.T.) ;
#8182 = ORIENTED_EDGE('',*,*,#6019,.T.) ;
#8183 = ORIENTED_EDGE('',*,*,#5947,.T.) ;
#8184 = ORIENTED_EDGE('',*,*,#6020,.T.) ;
#8185 = ORIENTED_EDGE('',*,*,#6021,.T.) ;
#8186 = ORIENTED_EDGE('',*,*,#5943,.T.) ;
#8187 = ORIENTED_EDGE('',*,*,#6022,.T.) ;
#8188 = ORIENTED_EDGE('',*,*,#6023,.T.) ;
#8189 = ORIENTED_EDGE('',*,*,#5939,.T.) ;
#8190 = ORIENTED_EDGE('',*,*,#6024,.T.) ;
#8191 = ORIENTED_EDGE('',*,*,#6025,.T.) ;
#8192 = ORIENTED_EDGE('',*,*,#5935,.T.) ;
#8193 = ORIENTED_EDGE('',*,*,#6026,.T.) ;
#8194 = ORIENTED_EDGE('',*,*,#6027,.T.) ;
#8195 = ORIENTED_EDGE('',*,*,#5931,.T.) ;
#8196 = ORIENTED_EDGE('',*,*,#6028,.T.) ;
#8197 = ORIENTED_EDGE('',*,*,#6029,.T.) ;
#8198 = ORIENTED_EDGE('',*,*,#5927,.T.) ;
#8199 = ORIENTED_EDGE('',*,*,#6030,.T.) ;
#8200 = ORIENTED_EDGE('',*,*,#6031,.T.) ;
#8201 = ORIENTED_EDGE('',*,*,#5923,.T.) ;
#8202 = ORIENTED_EDGE('',*,*,#6032,.T.) ;
#8203 = ORIENTED_EDGE('',*,*,#6033,.T.) ;
#8204 = ORIENTED_EDGE('',*,*,#5919,.T.) ;
#8205 = ORIENTED_EDGE('',*,*,#6034,.T.) ;
#8206 = ORIENTED_EDGE('',*,*,#6035,.T.) ;
#8207 = ORIENTED_EDGE('',*,*,#5915,.T.) ;
#8208 = ORIENTED_EDGE('',*,*,#6036,.T.) ;
#8209 = ORIENTED_EDGE('',*,*,#6037,.T.) ;
#8210 = ORIENTED_EDGE('',*,*,#5911,.T.) ;
#8211 = ORIENTED_EDGE('',*,*,#6038,.T.) ;
#8212 = ORIENTED_EDGE('',*,*,#6039,.T.) ;
#8213 = ORIENTED_EDGE('',*,*,#5907,.T.) ;
#8214 = ORIENTED_EDGE('',*,*,#6040,.T.) ;
#8215 = ORIENTED_EDGE('',*,*,#6041,.T.) ;
#8216 = ORIENTED_EDGE('',*,*,#5903,.T.) ;
#8217 = ORIENTED_EDGE('',*,*,#6042,.T.) ;
#8218 = ORIENTED_EDGE('',*,*,#5974,.F.) ;
#8219 = ORIENTED_EDGE('',*,*,#5961,.F.) ;
#8220 = ORIENTED_EDGE('',*,*,#6043,.F.) ;
#8221 = ORIENTED_EDGE('',*,*,#6044,.F.) ;
#8222 = ORIENTED_EDGE('',*,*,#5962,.F.) ;
#8223 = ORIENTED_EDGE('',*,*,#6044,.T.) ;
#8224 = ORIENTED_EDGE('',*,*,#6045,.F.) ;
#8225 = ORIENTED_EDGE('',*,*,#6012,.F.) ;
#8226 = ORIENTED_EDGE('',*,*,#5960,.F.) ;
#8227 = ORIENTED_EDGE('',*,*,#6013,.F.) ;
#8228 = ORIENTED_EDGE('',*,*,#6045,.T.) ;
#8229 = ORIENTED_EDGE('',*,*,#6043,.T.) ;
#8230 = ORIENTED_EDGE('',*,*,#5958,.F.) ;
#8231 = ORIENTED_EDGE('',*,*,#6046,.T.) ;
#8232 = ORIENTED_EDGE('',*,*,#6047,.F.) ;
#8233 = ORIENTED_EDGE('',*,*,#6014,.F.) ;
#8234 = ORIENTED_EDGE('',*,*,#6015,.F.) ;
#8235 = ORIENTED_EDGE('',*,*,#6047,.T.) ;
#8236 = ORIENTED_EDGE('',*,*,#6048,.T.) ;
#8237 = ORIENTED_EDGE('',*,*,#5956,.F.) ;
#8238 = ORIENTED_EDGE('',*,*,#5957,.F.) ;
#8239 = ORIENTED_EDGE('',*,*,#6048,.F.) ;
#8240 = ORIENTED_EDGE('',*,*,#6046,.F.) ;
#8241 = ORIENTED_EDGE('',*,*,#5953,.F.) ;
#8242 = ORIENTED_EDGE('',*,*,#6049,.F.) ;
#8243 = ORIENTED_EDGE('',*,*,#6050,.F.) ;
#8244 = ORIENTED_EDGE('',*,*,#5954,.F.) ;
#8245 = ORIENTED_EDGE('',*,*,#6050,.T.) ;
#8246 = ORIENTED_EDGE('',*,*,#6051,.F.) ;
#8247 = ORIENTED_EDGE('',*,*,#6016,.F.) ;
#8248 = ORIENTED_EDGE('',*,*,#5952,.F.) ;
#8249 = ORIENTED_EDGE('',*,*,#6017,.F.) ;
#8250 = ORIENTED_EDGE('',*,*,#6051,.T.) ;
#8251 = ORIENTED_EDGE('',*,*,#6049,.T.) ;
#8252 = ORIENTED_EDGE('',*,*,#5950,.F.) ;
#8253 = ORIENTED_EDGE('',*,*,#6052,.T.) ;
#8254 = ORIENTED_EDGE('',*,*,#6053,.F.) ;
#8255 = ORIENTED_EDGE('',*,*,#6018,.F.) ;
#8256 = ORIENTED_EDGE('',*,*,#6019,.F.) ;
#8257 = ORIENTED_EDGE('',*,*,#6053,.T.) ;
#8258 = ORIENTED_EDGE('',*,*,#6054,.T.) ;
#8259 = ORIENTED_EDGE('',*,*,#5948,.F.) ;
#8260 = ORIENTED_EDGE('',*,*,#5949,.F.) ;
#8261 = ORIENTED_EDGE('',*,*,#6054,.F.) ;
#8262 = ORIENTED_EDGE('',*,*,#6052,.F.) ;
#8263 = ORIENTED_EDGE('',*,*,#5945,.F.) ;
#8264 = ORIENTED_EDGE('',*,*,#6055,.F.) ;
#8265 = ORIENTED_EDGE('',*,*,#6056,.F.) ;
#8266 = ORIENTED_EDGE('',*,*,#5946,.F.) ;
#8267 = ORIENTED_EDGE('',*,*,#6056,.T.) ;
#8268 = ORIENTED_EDGE('',*,*,#6057,.F.) ;
#8269 = ORIENTED_EDGE('',*,*,#6020,.F.) ;
#8270 = ORIENTED_EDGE('',*,*,#5944,.F.) ;
#8271 = ORIENTED_EDGE('',*,*,#6021,.F.) ;
#8272 = ORIENTED_EDGE('',*,*,#6057,.T.) ;
#8273 = ORIENTED_EDGE('',*,*,#6055,.T.) ;
#8274 = ORIENTED_EDGE('',*,*,#5942,.F.) ;
#8275 = ORIENTED_EDGE('',*,*,#6058,.T.) ;
#8276 = ORIENTED_EDGE('',*,*,#6059,.F.) ;
#8277 = ORIENTED_EDGE('',*,*,#6022,.F.) ;
#8278 = ORIENTED_EDGE('',*,*,#6023,.F.) ;
#8279 = ORIENTED_EDGE('',*,*,#6059,.T.) ;
#8280 = ORIENTED_EDGE('',*,*,#6060,.T.) ;
#8281 = ORIENTED_EDGE('',*,*,#5940,.F.) ;
#8282 = ORIENTED_EDGE('',*,*,#5941,.F.) ;
#8283 = ORIENTED_EDGE('',*,*,#6060,.F.) ;
#8284 = ORIENTED_EDGE('',*,*,#6058,.F.) ;
#8285 = ORIENTED_EDGE('',*,*,#5937,.F.) ;
#8286 = ORIENTED_EDGE('',*,*,#6061,.F.) ;
#8287 = ORIENTED_EDGE('',*,*,#6062,.F.) ;
#8288 = ORIENTED_EDGE('',*,*,#5938,.F.) ;
#8289 = ORIENTED_EDGE('',*,*,#6062,.T.) ;
#8290 = ORIENTED_EDGE('',*,*,#6063,.F.) ;
#8291 = ORIENTED_EDGE('',*,*,#6024,.F.) ;
#8292 = ORIENTED_EDGE('',*,*,#5936,.F.) ;
#8293 = ORIENTED_EDGE('',*,*,#6025,.F.) ;
#8294 = ORIENTED_EDGE('',*,*,#6063,.T.) ;
#8295 = ORIENTED_EDGE('',*,*,#6061,.T.) ;
#8296 = ORIENTED_EDGE('',*,*,#5934,.F.) ;
#8297 = ORIENTED_EDGE('',*,*,#6064,.T.) ;
#8298 = ORIENTED_EDGE('',*,*,#6065,.F.) ;
#8299 = ORIENTED_EDGE('',*,*,#6026,.F.) ;
#8300 = ORIENTED_EDGE('',*,*,#6027,.F.) ;
#8301 = ORIENTED_EDGE('',*,*,#6065,.T.) ;
#8302 = ORIENTED_EDGE('',*,*,#6066,.T.) ;
#8303 = ORIENTED_EDGE('',*,*,#5932,.F.) ;
#8304 = ORIENTED_EDGE('',*,*,#5933,.F.) ;
#8305 = ORIENTED_EDGE('',*,*,#6066,.F.) ;
#8306 = ORIENTED_EDGE('',*,*,#6064,.F.) ;
#8307 = ORIENTED_EDGE('',*,*,#5929,.F.) ;
#8308 = ORIENTED_EDGE('',*,*,#6067,.F.) ;
#8309 = ORIENTED_EDGE('',*,*,#6068,.F.) ;
#8310 = ORIENTED_EDGE('',*,*,#5930,.F.) ;
#8311 = ORIENTED_EDGE('',*,*,#6068,.T.) ;
#8312 = ORIENTED_EDGE('',*,*,#6069,.F.) ;
#8313 = ORIENTED_EDGE('',*,*,#6028,.F.) ;
#8314 = ORIENTED_EDGE('',*,*,#5928,.F.) ;
#8315 = ORIENTED_EDGE('',*,*,#6029,.F.) ;
#8316 = ORIENTED_EDGE('',*,*,#6069,.T.) ;
#8317 = ORIENTED_EDGE('',*,*,#6067,.T.) ;
#8318 = ORIENTED_EDGE('',*,*,#5926,.F.) ;
#8319 = ORIENTED_EDGE('',*,*,#6070,.T.) ;
#8320 = ORIENTED_EDGE('',*,*,#6071,.F.) ;
#8321 = ORIENTED_EDGE('',*,*,#6030,.F.) ;
#8322 = ORIENTED_EDGE('',*,*,#6031,.F.) ;
#8323 = ORIENTED_EDGE('',*,*,#6071,.T.) ;
#8324 = ORIENTED_EDGE('',*,*,#6072,.T.) ;
#8325 = ORIENTED_EDGE('',*,*,#5924,.F.) ;
#8326 = ORIENTED_EDGE('',*,*,#5925,.F.) ;
#8327 = ORIENTED_EDGE('',*,*,#6072,.F.) ;
#8328 = ORIENTED_EDGE('',*,*,#6070,.F.) ;
#8329 = ORIENTED_EDGE('',*,*,#5921,.F.) ;
#8330 = ORIENTED_EDGE('',*,*,#6073,.F.) ;
#8331 = ORIENTED_EDGE('',*,*,#6074,.F.) ;
#8332 = ORIENTED_EDGE('',*,*,#5922,.F.) ;
#8333 = ORIENTED_EDGE('',*,*,#6074,.T.) ;
#8334 = ORIENTED_EDGE('',*,*,#6075,.F.) ;
#8335 = ORIENTED_EDGE('',*,*,#6032,.F.) ;
#8336 = ORIENTED_EDGE('',*,*,#5920,.F.) ;
#8337 = ORIENTED_EDGE('',*,*,#6033,.F.) ;
#8338 = ORIENTED_EDGE('',*,*,#6075,.T.) ;
#8339 = ORIENTED_EDGE('',*,*,#6073,.T.) ;
#8340 = ORIENTED_EDGE('',*,*,#5918,.F.) ;
#8341 = ORIENTED_EDGE('',*,*,#6076,.T.) ;
#8342 = ORIENTED_EDGE('',*,*,#6077,.F.) ;
#8343 = ORIENTED_EDGE('',*,*,#6034,.F.) ;
#8344 = ORIENTED_EDGE('',*,*,#6035,.F.) ;
#8345 = ORIENTED_EDGE('',*,*,#6077,.T.) ;
#8346 = ORIENTED_EDGE('',*,*,#6078,.T.) ;
#8347 = ORIENTED_EDGE('',*,*,#5916,.F.) ;
#8348 = ORIENTED_EDGE('',*,*,#5917,.F.) ;
#8349 = ORIENTED_EDGE('',*,*,#6078,.F.) ;
#8350 = ORIENTED_EDGE('',*,*,#6076,.F.) ;
#8351 = ORIENTED_EDGE('',*,*,#5913,.F.) ;
#8352 = ORIENTED_EDGE('',*,*,#6079,.F.) ;
#8353 = ORIENTED_EDGE('',*,*,#6080,.F.) ;
#8354 = ORIENTED_EDGE('',*,*,#5914,.F.) ;
#8355 = ORIENTED_EDGE('',*,*,#6080,.T.) ;
#8356 = ORIENTED_EDGE('',*,*,#6081,.F.) ;
#8357 = ORIENTED_EDGE('',*,*,#6036,.F.) ;
#8358 = ORIENTED_EDGE('',*,*,#5912,.F.) ;
#8359 = ORIENTED_EDGE('',*,*,#6037,.F.) ;
#8360 = ORIENTED_EDGE('',*,*,#6081,.T.) ;
#8361 = ORIENTED_EDGE('',*,*,#6079,.T.) ;
#8362 = ORIENTED_EDGE('',*,*,#5910,.F.) ;
#8363 = ORIENTED_EDGE('',*,*,#6082,.T.) ;
#8364 = ORIENTED_EDGE('',*,*,#6083,.F.) ;
#8365 = ORIENTED_EDGE('',*,*,#6038,.F.) ;
#8366 = ORIENTED_EDGE('',*,*,#6039,.F.) ;
#8367 = ORIENTED_EDGE('',*,*,#6083,.T.) ;
#8368 = ORIENTED_EDGE('',*,*,#6084,.T.) ;
#8369 = ORIENTED_EDGE('',*,*,#5908,.F.) ;
#8370 = ORIENTED_EDGE('',*,*,#5909,.F.) ;
#8371 = ORIENTED_EDGE('',*,*,#6084,.F.) ;
#8372 = ORIENTED_EDGE('',*,*,#6082,.F.) ;
#8373 = ORIENTED_EDGE('',*,*,#5905,.F.) ;
#8374 = ORIENTED_EDGE('',*,*,#6085,.F.) ;
#8375 = ORIENTED_EDGE('',*,*,#6086,.F.) ;
#8376 = ORIENTED_EDGE('',*,*,#5906,.F.) ;
#8377 = ORIENTED_EDGE('',*,*,#6086,.T.) ;
#8378 = ORIENTED_EDGE('',*,*,#6087,.F.) ;
#8379 = ORIENTED_EDGE('',*,*,#6040,.F.) ;
#8380 = ORIENTED_EDGE('',*,*,#5904,.F.) ;
#8381 = ORIENTED_EDGE('',*,*,#6041,.F.) ;
#8382 = ORIENTED_EDGE('',*,*,#6087,.T.) ;
#8383 = ORIENTED_EDGE('',*,*,#6085,.T.) ;
#8384 = ORIENTED_EDGE('',*,*,#5902,.F.) ;
#8385 = ORIENTED_EDGE('',*,*,#6088,.T.) ;
#8386 = ORIENTED_EDGE('',*,*,#6089,.F.) ;
#8387 = ORIENTED_EDGE('',*,*,#6042,.F.) ;
#8388 = ORIENTED_EDGE('',*,*,#5975,.F.) ;
#8389 = ORIENTED_EDGE('',*,*,#6089,.T.) ;
#8390 = ORIENTED_EDGE('',*,*,#6090,.T.) ;
#8391 = ORIENTED_EDGE('',*,*,#5897,.F.) ;
#8392 = ORIENTED_EDGE('',*,*,#5898,.F.) ;
#8393 = ORIENTED_EDGE('',*,*,#6090,.F.) ;
#8394 = ORIENTED_EDGE('',*,*,#6088,.F.) ;
#8395 = ORIENTED_EDGE('',*,*,#5901,.F.) ;
#8396 = ORIENTED_EDGE('',*,*,#5894,.F.) ;
#8397 = ORIENTED_EDGE('',*,*,#6091,.F.) ;
#8398 = ORIENTED_EDGE('',*,*,#6092,.F.) ;
#8399 = ORIENTED_EDGE('',*,*,#5895,.F.) ;
#8400 = ORIENTED_EDGE('',*,*,#6092,.T.) ;
#8401 = ORIENTED_EDGE('',*,*,#6093,.F.) ;
#8402 = ORIENTED_EDGE('',*,*,#5976,.F.) ;
#8403 = ORIENTED_EDGE('',*,*,#5893,.F.) ;
#8404 = ORIENTED_EDGE('',*,*,#5977,.F.) ;
#8405 = ORIENTED_EDGE('',*,*,#6093,.T.) ;
#8406 = ORIENTED_EDGE('',*,*,#6091,.T.) ;
#8407 = ORIENTED_EDGE('',*,*,#5891,.F.) ;
#8408 = ORIENTED_EDGE('',*,*,#6094,.T.) ;
#8409 = ORIENTED_EDGE('',*,*,#6095,.F.) ;
#8410 = ORIENTED_EDGE('',*,*,#5978,.F.) ;
#8411 = ORIENTED_EDGE('',*,*,#5979,.F.) ;
#8412 = ORIENTED_EDGE('',*,*,#6095,.T.) ;
#8413 = ORIENTED_EDGE('',*,*,#6096,.T.) ;
#8414 = ORIENTED_EDGE('',*,*,#5889,.F.) ;
#8415 = ORIENTED_EDGE('',*,*,#5890,.F.) ;
#8416 = ORIENTED_EDGE('',*,*,#6096,.F.) ;
#8417 = ORIENTED_EDGE('',*,*,#6094,.F.) ;
#8418 = ORIENTED_EDGE('',*,*,#5886,.F.) ;
#8419 = ORIENTED_EDGE('',*,*,#6097,.F.) ;
#8420 = ORIENTED_EDGE('',*,*,#6098,.F.) ;
#8421 = ORIENTED_EDGE('',*,*,#5887,.F.) ;
#8422 = ORIENTED_EDGE('',*,*,#6098,.T.) ;
#8423 = ORIENTED_EDGE('',*,*,#6099,.F.) ;
#8424 = ORIENTED_EDGE('',*,*,#5980,.F.) ;
#8425 = ORIENTED_EDGE('',*,*,#5885,.F.) ;
#8426 = ORIENTED_EDGE('',*,*,#5981,.F.) ;
#8427 = ORIENTED_EDGE('',*,*,#6099,.T.) ;
#8428 = ORIENTED_EDGE('',*,*,#6097,.T.) ;
#8429 = ORIENTED_EDGE('',*,*,#5883,.F.) ;
#8430 = ORIENTED_EDGE('',*,*,#6100,.T.) ;
#8431 = ORIENTED_EDGE('',*,*,#6101,.F.) ;
#8432 = ORIENTED_EDGE('',*,*,#5982,.F.) ;
#8433 = ORIENTED_EDGE('',*,*,#5983,.F.) ;
#8434 = ORIENTED_EDGE('',*,*,#6101,.T.) ;
#8435 = ORIENTED_EDGE('',*,*,#6102,.T.) ;
#8436 = ORIENTED_EDGE('',*,*,#5881,.F.) ;
#8437 = ORIENTED_EDGE('',*,*,#5882,.F.) ;
#8438 = ORIENTED_EDGE('',*,*,#6102,.F.) ;
#8439 = ORIENTED_EDGE('',*,*,#6100,.F.) ;
#8440 = ORIENTED_EDGE('',*,*,#5878,.F.) ;
#8441 = ORIENTED_EDGE('',*,*,#6103,.F.) ;
#8442 = ORIENTED_EDGE('',*,*,#6104,.F.) ;
#8443 = ORIENTED_EDGE('',*,*,#5879,.F.) ;
#8444 = ORIENTED_EDGE('',*,*,#6104,.T.) ;
#8445 = ORIENTED_EDGE('',*,*,#6105,.F.) ;
#8446 = ORIENTED_EDGE('',*,*,#5984,.F.) ;
#8447 = ORIENTED_EDGE('',*,*,#5877,.F.) ;
#8448 = ORIENTED_EDGE('',*,*,#5985,.F.) ;
#8449 = ORIENTED_EDGE('',*,*,#6105,.T.) ;
#8450 = ORIENTED_EDGE('',*,*,#6103,.T.) ;
#8451 = ORIENTED_EDGE('',*,*,#5875,.F.) ;
#8452 = ORIENTED_EDGE('',*,*,#6106,.T.) ;
#8453 = ORIENTED_EDGE('',*,*,#6107,.F.) ;
#8454 = ORIENTED_EDGE('',*,*,#5986,.F.) ;
#8455 = ORIENTED_EDGE('',*,*,#5987,.F.) ;
#8456 = ORIENTED_EDGE('',*,*,#6107,.T.) ;
#8457 = ORIENTED_EDGE('',*,*,#6108,.T.) ;
#8458 = ORIENTED_EDGE('',*,*,#5873,.F.) ;
#8459 = ORIENTED_EDGE('',*,*,#5874,.F.) ;
#8460 = ORIENTED_EDGE('',*,*,#6108,.F.) ;
#8461 = ORIENTED_EDGE('',*,*,#6106,.F.) ;
#8462 = ORIENTED_EDGE('',*,*,#5870,.F.) ;
#8463 = ORIENTED_EDGE('',*,*,#6109,.F.) ;
#8464 = ORIENTED_EDGE('',*,*,#6110,.F.) ;
#8465 = ORIENTED_EDGE('',*,*,#5871,.F.) ;
#8466 = ORIENTED_EDGE('',*,*,#6110,.T.) ;
#8467 = ORIENTED_EDGE('',*,*,#6111,.F.) ;
#8468 = ORIENTED_EDGE('',*,*,#5988,.F.) ;
#8469 = ORIENTED_EDGE('',*,*,#5869,.F.) ;
#8470 = ORIENTED_EDGE('',*,*,#5989,.F.) ;
#8471 = ORIENTED_EDGE('',*,*,#6111,.T.) ;
#8472 = ORIENTED_EDGE('',*,*,#6109,.T.) ;
#8473 = ORIENTED_EDGE('',*,*,#5867,.F.) ;
#8474 = ORIENTED_EDGE('',*,*,#6112,.T.) ;
#8475 = ORIENTED_EDGE('',*,*,#6113,.F.) ;
#8476 = ORIENTED_EDGE('',*,*,#5990,.F.) ;
#8477 = ORIENTED_EDGE('',*,*,#5991,.F.) ;
#8478 = ORIENTED_EDGE('',*,*,#6113,.T.) ;
#8479 = ORIENTED_EDGE('',*,*,#6114,.T.) ;
#8480 = ORIENTED_EDGE('',*,*,#5865,.F.) ;
#8481 = ORIENTED_EDGE('',*,*,#5866,.F.) ;
#8482 = ORIENTED_EDGE('',*,*,#6114,.F.) ;
#8483 = ORIENTED_EDGE('',*,*,#6112,.F.) ;
#8484 = ORIENTED_EDGE('',*,*,#5862,.F.) ;
#8485 = ORIENTED_EDGE('',*,*,#6115,.F.) ;
#8486 = ORIENTED_EDGE('',*,*,#6116,.F.) ;
#8487 = ORIENTED_EDGE('',*,*,#5863,.F.) ;
#8488 = ORIENTED_EDGE('',*,*,#6116,.T.) ;
#8489 = ORIENTED_EDGE('',*,*,#6117,.F.) ;
#8490 = ORIENTED_EDGE('',*,*,#5992,.F.) ;
#8491 = ORIENTED_EDGE('',*,*,#5861,.F.) ;
#8492 = ORIENTED_EDGE('',*,*,#5993,.F.) ;
#8493 = ORIENTED_EDGE('',*,*,#6117,.T.) ;
#8494 = ORIENTED_EDGE('',*,*,#6115,.T.) ;
#8495 = ORIENTED_EDGE('',*,*,#5859,.F.) ;
#8496 = ORIENTED_EDGE('',*,*,#6118,.T.) ;
#8497 = ORIENTED_EDGE('',*,*,#6119,.F.) ;
#8498 = ORIENTED_EDGE('',*,*,#5994,.F.) ;
#8499 = ORIENTED_EDGE('',*,*,#5995,.F.) ;
#8500 = ORIENTED_EDGE('',*,*,#6119,.T.) ;
#8501 = ORIENTED_EDGE('',*,*,#6120,.T.) ;
#8502 = ORIENTED_EDGE('',*,*,#5857,.F.) ;
#8503 = ORIENTED_EDGE('',*,*,#5858,.F.) ;
#8504 = ORIENTED_EDGE('',*,*,#6120,.F.) ;
#8505 = ORIENTED_EDGE('',*,*,#6118,.F.) ;
#8506 = ORIENTED_EDGE('',*,*,#5854,.F.) ;
#8507 = ORIENTED_EDGE('',*,*,#6121,.F.) ;
#8508 = ORIENTED_EDGE('',*,*,#6122,.F.) ;
#8509 = ORIENTED_EDGE('',*,*,#5855,.F.) ;
#8510 = ORIENTED_EDGE('',*,*,#6122,.T.) ;
#8511 = ORIENTED_EDGE('',*,*,#6123,.F.) ;
#8512 = ORIENTED_EDGE('',*,*,#5996,.F.) ;
#8513 = ORIENTED_EDGE('',*,*,#5853,.F.) ;
#8514 = ORIENTED_EDGE('',*,*,#5997,.F.) ;
#8515 = ORIENTED_EDGE('',*,*,#6123,.T.) ;
#8516 = ORIENTED_EDGE('',*,*,#6121,.T.) ;
#8517 = ORIENTED_EDGE('',*,*,#5851,.F.) ;
#8518 = ORIENTED_EDGE('',*,*,#6124,.T.) ;
#8519 = ORIENTED_EDGE('',*,*,#6125,.F.) ;
#8520 = ORIENTED_EDGE('',*,*,#5998,.F.) ;
#8521 = ORIENTED_EDGE('',*,*,#5999,.F.) ;
#8522 = ORIENTED_EDGE('',*,*,#6125,.T.) ;
#8523 = ORIENTED_EDGE('',*,*,#6126,.T.) ;
#8524 = ORIENTED_EDGE('',*,*,#5849,.F.) ;
#8525 = ORIENTED_EDGE('',*,*,#5850,.F.) ;
#8526 = ORIENTED_EDGE('',*,*,#6126,.F.) ;
#8527 = ORIENTED_EDGE('',*,*,#6124,.F.) ;
#8528 = ORIENTED_EDGE('',*,*,#5846,.F.) ;
#8529 = ORIENTED_EDGE('',*,*,#6127,.F.) ;
#8530 = ORIENTED_EDGE('',*,*,#6128,.F.) ;
#8531 = ORIENTED_EDGE('',*,*,#5847,.F.) ;
#8532 = ORIENTED_EDGE('',*,*,#6128,.T.) ;
#8533 = ORIENTED_EDGE('',*,*,#6129,.F.) ;
#8534 = ORIENTED_EDGE('',*,*,#6000,.F.) ;
#8535 = ORIENTED_EDGE('',*,*,#5845,.F.) ;
#8536 = ORIENTED_EDGE('',*,*,#6001,.F.) ;
#8537 = ORIENTED_EDGE('',*,*,#6129,.T.) ;
#8538 = ORIENTED_EDGE('',*,*,#6127,.T.) ;
#8539 = ORIENTED_EDGE('',*,*,#5843,.F.) ;
#8540 = ORIENTED_EDGE('',*,*,#6130,.T.) ;
#8541 = ORIENTED_EDGE('',*,*,#6131,.F.) ;
#8542 = ORIENTED_EDGE('',*,*,#6002,.F.) ;
#8543 = ORIENTED_EDGE('',*,*,#6003,.F.) ;
#8544 = ORIENTED_EDGE('',*,*,#6131,.T.) ;
#8545 = ORIENTED_EDGE('',*,*,#6132,.T.) ;
#8546 = ORIENTED_EDGE('',*,*,#5841,.F.) ;
#8547 = ORIENTED_EDGE('',*,*,#5842,.F.) ;
#8548 = ORIENTED_EDGE('',*,*,#6132,.F.) ;
#8549 = ORIENTED_EDGE('',*,*,#6130,.F.) ;
#8550 = ORIENTED_EDGE('',*,*,#5838,.F.) ;
#8551 = ORIENTED_EDGE('',*,*,#6133,.F.) ;
#8552 = ORIENTED_EDGE('',*,*,#6134,.F.) ;
#8553 = ORIENTED_EDGE('',*,*,#5839,.F.) ;
#8554 = ORIENTED_EDGE('',*,*,#6134,.T.) ;
#8555 = ORIENTED_EDGE('',*,*,#6135,.F.) ;
#8556 = ORIENTED_EDGE('',*,*,#6004,.F.) ;
#8557 = ORIENTED_EDGE('',*,*,#5837,.F.) ;
#8558 = ORIENTED_EDGE('',*,*,#6005,.F.) ;
#8559 = ORIENTED_EDGE('',*,*,#6135,.T.) ;
#8560 = ORIENTED_EDGE('',*,*,#6133,.T.) ;
#8561 = ORIENTED_EDGE('',*,*,#5835,.F.) ;
#8562 = ORIENTED_EDGE('',*,*,#6136,.T.) ;
#8563 = ORIENTED_EDGE('',*,*,#6137,.F.) ;
#8564 = ORIENTED_EDGE('',*,*,#6006,.F.) ;
#8565 = ORIENTED_EDGE('',*,*,#6007,.F.) ;
#8566 = ORIENTED_EDGE('',*,*,#6137,.T.) ;
#8567 = ORIENTED_EDGE('',*,*,#6138,.T.) ;
#8568 = ORIENTED_EDGE('',*,*,#5833,.F.) ;
#8569 = ORIENTED_EDGE('',*,*,#5834,.F.) ;
#8570 = ORIENTED_EDGE('',*,*,#6138,.F.) ;
#8571 = ORIENTED_EDGE('',*,*,#6136,.F.) ;
#8572 = ORIENTED_EDGE('',*,*,#5830,.F.) ;
#8573 = ORIENTED_EDGE('',*,*,#6139,.F.) ;
#8574 = ORIENTED_EDGE('',*,*,#6140,.F.) ;
#8575 = ORIENTED_EDGE('',*,*,#5831,.F.) ;
#8576 = ORIENTED_EDGE('',*,*,#6140,.T.) ;
#8577 = ORIENTED_EDGE('',*,*,#6141,.F.) ;
#8578 = ORIENTED_EDGE('',*,*,#6008,.F.) ;
#8579 = ORIENTED_EDGE('',*,*,#5829,.F.) ;
#8580 = ORIENTED_EDGE('',*,*,#6009,.F.) ;
#8581 = ORIENTED_EDGE('',*,*,#6141,.T.) ;
#8582 = ORIENTED_EDGE('',*,*,#6139,.T.) ;
#8583 = ORIENTED_EDGE('',*,*,#5827,.F.) ;
#8584 = ORIENTED_EDGE('',*,*,#6142,.T.) ;
#8585 = ORIENTED_EDGE('',*,*,#6143,.F.) ;
#8586 = ORIENTED_EDGE('',*,*,#6010,.F.) ;
#8587 = ORIENTED_EDGE('',*,*,#6011,.F.) ;
#8588 = ORIENTED_EDGE('',*,*,#6143,.T.) ;
#8589 = ORIENTED_EDGE('',*,*,#6144,.T.) ;
#8590 = ORIENTED_EDGE('',*,*,#5825,.F.) ;
#8591 = ORIENTED_EDGE('',*,*,#5826,.F.) ;
#8592 = ORIENTED_EDGE('',*,*,#6144,.F.) ;
#8593 = ORIENTED_EDGE('',*,*,#6142,.F.) ;
#8594 = ORIENTED_EDGE('',*,*,#5813,.T.) ;
#8595 = ORIENTED_EDGE('',*,*,#6145,.T.) ;
#8596 = ORIENTED_EDGE('',*,*,#5900,.T.) ;
#8597 = ORIENTED_EDGE('',*,*,#6145,.F.) ;
#8598 = ORIENTED_EDGE('',*,*,#5973,.F.) ;
#8599 = ORIENTED_EDGE('',*,*,#6146,.T.) ;
#8600 = ORIENTED_EDGE('',*,*,#6146,.F.) ;
#8601 = ORIENTED_EDGE('',*,*,#6147,.T.) ;
#8602 = ORIENTED_EDGE('',*,*,#6148,.F.) ;
#8603 = ORIENTED_EDGE('',*,*,#6149,.T.) ;
#8604 = ORIENTED_EDGE('',*,*,#6150,.F.) ;
#8605 = ORIENTED_EDGE('',*,*,#6151,.F.) ;
#8606 = ORIENTED_EDGE('',*,*,#6152,.T.) ;
#8607 = ORIENTED_EDGE('',*,*,#6153,.F.) ;
#8608 = ORIENTED_EDGE('',*,*,#6154,.F.) ;
#8609 = ORIENTED_EDGE('',*,*,#6155,.T.) ;
#8610 = ORIENTED_EDGE('',*,*,#6156,.F.) ;
#8611 = ORIENTED_EDGE('',*,*,#6157,.F.) ;
#8612 = ORIENTED_EDGE('',*,*,#6158,.T.) ;
#8613 = ORIENTED_EDGE('',*,*,#6159,.F.) ;
#8614 = ORIENTED_EDGE('',*,*,#6160,.F.) ;
#8615 = ORIENTED_EDGE('',*,*,#6161,.T.) ;
#8616 = ORIENTED_EDGE('',*,*,#6162,.F.) ;
#8617 = ORIENTED_EDGE('',*,*,#6163,.F.) ;
#8618 = ORIENTED_EDGE('',*,*,#6164,.T.) ;
#8619 = ORIENTED_EDGE('',*,*,#6165,.F.) ;
#8620 = ORIENTED_EDGE('',*,*,#6147,.F.) ;
#8621 = ORIENTED_EDGE('',*,*,#6166,.F.) ;
#8622 = ORIENTED_EDGE('',*,*,#6155,.F.) ;
#8623 = ORIENTED_EDGE('',*,*,#6167,.F.) ;
#8624 = ORIENTED_EDGE('',*,*,#6168,.F.) ;
#8625 = ORIENTED_EDGE('',*,*,#6169,.F.) ;
#8626 = ORIENTED_EDGE('',*,*,#6158,.F.) ;
#8627 = ORIENTED_EDGE('',*,*,#6170,.F.) ;
#8628 = ORIENTED_EDGE('',*,*,#6171,.F.) ;
#8629 = ORIENTED_EDGE('',*,*,#6172,.F.) ;
#8630 = ORIENTED_EDGE('',*,*,#6173,.F.) ;
#8631 = ORIENTED_EDGE('',*,*,#6174,.F.) ;
#8632 = ORIENTED_EDGE('',*,*,#6152,.F.) ;
#8633 = ORIENTED_EDGE('',*,*,#6175,.F.) ;
#8634 = ORIENTED_EDGE('',*,*,#6161,.F.) ;
#8635 = ORIENTED_EDGE('',*,*,#6176,.F.) ;
#8636 = ORIENTED_EDGE('',*,*,#6177,.F.) ;
#8637 = ORIENTED_EDGE('',*,*,#6178,.F.) ;
#8638 = ORIENTED_EDGE('',*,*,#6179,.F.) ;
#8639 = ORIENTED_EDGE('',*,*,#6180,.F.) ;
#8640 = ORIENTED_EDGE('',*,*,#6149,.F.) ;
#8641 = ORIENTED_EDGE('',*,*,#6181,.F.) ;
#8642 = ORIENTED_EDGE('',*,*,#6182,.F.) ;
#8643 = ORIENTED_EDGE('',*,*,#6183,.F.) ;
#8644 = ORIENTED_EDGE('',*,*,#6164,.F.) ;
#8645 = ORIENTED_EDGE('',*,*,#6162,.T.) ;
#8646 = ORIENTED_EDGE('',*,*,#6175,.T.) ;
#8647 = ORIENTED_EDGE('',*,*,#6184,.F.) ;
#8648 = ORIENTED_EDGE('',*,*,#6176,.T.) ;
#8649 = ORIENTED_EDGE('',*,*,#6160,.T.) ;
#8650 = ORIENTED_EDGE('',*,*,#6185,.T.) ;
#8651 = ORIENTED_EDGE('',*,*,#6186,.T.) ;
#8652 = ORIENTED_EDGE('',*,*,#6187,.F.) ;
#8653 = ORIENTED_EDGE('',*,*,#6159,.T.) ;
#8654 = ORIENTED_EDGE('',*,*,#6169,.T.) ;
#8655 = ORIENTED_EDGE('',*,*,#6188,.F.) ;
#8656 = ORIENTED_EDGE('',*,*,#6170,.T.) ;
#8657 = ORIENTED_EDGE('',*,*,#6157,.T.) ;
#8658 = ORIENTED_EDGE('',*,*,#6189,.T.) ;
#8659 = ORIENTED_EDGE('',*,*,#6190,.T.) ;
#8660 = ORIENTED_EDGE('',*,*,#6185,.F.) ;
#8661 = ORIENTED_EDGE('',*,*,#6156,.T.) ;
#8662 = ORIENTED_EDGE('',*,*,#6166,.T.) ;
#8663 = ORIENTED_EDGE('',*,*,#6191,.F.) ;
#8664 = ORIENTED_EDGE('',*,*,#6167,.T.) ;
#8665 = ORIENTED_EDGE('',*,*,#6154,.T.) ;
#8666 = ORIENTED_EDGE('',*,*,#6192,.T.) ;
#8667 = ORIENTED_EDGE('',*,*,#6193,.T.) ;
#8668 = ORIENTED_EDGE('',*,*,#6189,.F.) ;
#8669 = ORIENTED_EDGE('',*,*,#6168,.T.) ;
#8670 = ORIENTED_EDGE('',*,*,#6191,.T.) ;
#8671 = ORIENTED_EDGE('',*,*,#6171,.T.) ;
#8672 = ORIENTED_EDGE('',*,*,#6188,.T.) ;
#8673 = ORIENTED_EDGE('',*,*,#6173,.T.) ;
#8674 = ORIENTED_EDGE('',*,*,#6194,.T.) ;
#8675 = ORIENTED_EDGE('',*,*,#6177,.T.) ;
#8676 = ORIENTED_EDGE('',*,*,#6184,.T.) ;
#8677 = ORIENTED_EDGE('',*,*,#6179,.T.) ;
#8678 = ORIENTED_EDGE('',*,*,#6195,.T.) ;
#8679 = ORIENTED_EDGE('',*,*,#6182,.T.) ;
#8680 = ORIENTED_EDGE('',*,*,#6196,.T.) ;
#8681 = ORIENTED_EDGE('',*,*,#6197,.F.) ;
#8682 = ORIENTED_EDGE('',*,*,#6198,.T.) ;
#8683 = ORIENTED_EDGE('',*,*,#6193,.F.) ;
#8684 = ORIENTED_EDGE('',*,*,#6199,.T.) ;
#8685 = ORIENTED_EDGE('',*,*,#6190,.F.) ;
#8686 = ORIENTED_EDGE('',*,*,#6200,.T.) ;
#8687 = ORIENTED_EDGE('',*,*,#6186,.F.) ;
#8688 = ORIENTED_EDGE('',*,*,#6201,.T.) ;
#8689 = ORIENTED_EDGE('',*,*,#6202,.F.) ;
#8690 = ORIENTED_EDGE('',*,*,#6203,.T.) ;
#8691 = ORIENTED_EDGE('',*,*,#6204,.F.) ;
#8692 = ORIENTED_EDGE('',*,*,#6205,.T.) ;
#8693 = ORIENTED_EDGE('',*,*,#6200,.F.) ;
#8694 = ORIENTED_EDGE('',*,*,#6199,.F.) ;
#8695 = ORIENTED_EDGE('',*,*,#6198,.F.) ;
#8696 = ORIENTED_EDGE('',*,*,#6205,.F.) ;
#8697 = ORIENTED_EDGE('',*,*,#6206,.T.) ;
#8698 = ORIENTED_EDGE('',*,*,#6206,.F.) ;
#8699 = ORIENTED_EDGE('',*,*,#6203,.F.) ;
#8700 = ORIENTED_EDGE('',*,*,#6201,.F.) ;
#8701 = ORIENTED_EDGE('',*,*,#6151,.T.) ;
#8702 = ORIENTED_EDGE('',*,*,#6207,.T.) ;
#8703 = ORIENTED_EDGE('',*,*,#6197,.T.) ;
#8704 = ORIENTED_EDGE('',*,*,#6192,.F.) ;
#8705 = ORIENTED_EDGE('',*,*,#6153,.T.) ;
#8706 = ORIENTED_EDGE('',*,*,#6174,.T.) ;
#8707 = ORIENTED_EDGE('',*,*,#6194,.F.) ;
#8708 = ORIENTED_EDGE('',*,*,#6172,.T.) ;
#8709 = ORIENTED_EDGE('',*,*,#6148,.T.) ;
#8710 = ORIENTED_EDGE('',*,*,#6208,.T.) ;
#8711 = ORIENTED_EDGE('',*,*,#6204,.T.) ;
#8712 = ORIENTED_EDGE('',*,*,#6207,.F.) ;
#8713 = ORIENTED_EDGE('',*,*,#6150,.T.) ;
#8714 = ORIENTED_EDGE('',*,*,#6180,.T.) ;
#8715 = ORIENTED_EDGE('',*,*,#6195,.F.) ;
#8716 = ORIENTED_EDGE('',*,*,#6178,.T.) ;
#8717 = ORIENTED_EDGE('',*,*,#6163,.T.) ;
#8718 = ORIENTED_EDGE('',*,*,#6187,.T.) ;
#8719 = ORIENTED_EDGE('',*,*,#6202,.T.) ;
#8720 = ORIENTED_EDGE('',*,*,#6208,.F.) ;
#8721 = ORIENTED_EDGE('',*,*,#6165,.T.) ;
#8722 = ORIENTED_EDGE('',*,*,#6183,.T.) ;
#8723 = ORIENTED_EDGE('',*,*,#6196,.F.) ;
#8724 = ORIENTED_EDGE('',*,*,#6181,.T.) ;
#8725 = ORIENTED_EDGE('',*,*,#6209,.F.) ;
#8726 = ORIENTED_EDGE('',*,*,#6210,.T.) ;
#8727 = ORIENTED_EDGE('',*,*,#6211,.F.) ;
#8728 = ORIENTED_EDGE('',*,*,#6210,.F.) ;
#8729 = ORIENTED_EDGE('',*,*,#6212,.F.) ;
#8730 = ORIENTED_EDGE('',*,*,#6213,.T.) ;
#8731 = ORIENTED_EDGE('',*,*,#6214,.F.) ;
#8732 = ORIENTED_EDGE('',*,*,#6213,.F.) ;
#8733 = ORIENTED_EDGE('',*,*,#6215,.F.) ;
#8734 = ORIENTED_EDGE('',*,*,#6216,.F.) ;
#8735 = ORIENTED_EDGE('',*,*,#6217,.F.) ;
#8736 = ORIENTED_EDGE('',*,*,#6218,.T.) ;
#8737 = ORIENTED_EDGE('',*,*,#6219,.T.) ;
#8738 = ORIENTED_EDGE('',*,*,#6220,.F.) ;
#8739 = ORIENTED_EDGE('',*,*,#6221,.F.) ;
#8740 = ORIENTED_EDGE('',*,*,#6222,.T.) ;
#8741 = ORIENTED_EDGE('',*,*,#6223,.T.) ;
#8742 = ORIENTED_EDGE('',*,*,#6222,.F.) ;
#8743 = ORIENTED_EDGE('',*,*,#6224,.T.) ;
#8744 = ORIENTED_EDGE('',*,*,#6217,.T.) ;
#8745 = ORIENTED_EDGE('',*,*,#6225,.F.) ;
#8746 = ORIENTED_EDGE('',*,*,#6226,.F.) ;
#8747 = ORIENTED_EDGE('',*,*,#6227,.T.) ;
#8748 = ORIENTED_EDGE('',*,*,#6226,.T.) ;
#8749 = ORIENTED_EDGE('',*,*,#6228,.F.) ;
#8750 = ORIENTED_EDGE('',*,*,#6229,.F.) ;
#8751 = ORIENTED_EDGE('',*,*,#6230,.T.) ;
#8752 = ORIENTED_EDGE('',*,*,#6229,.T.) ;
#8753 = ORIENTED_EDGE('',*,*,#6231,.F.) ;
#8754 = ORIENTED_EDGE('',*,*,#6219,.F.) ;
#8755 = ORIENTED_EDGE('',*,*,#6232,.F.) ;
#8756 = ORIENTED_EDGE('',*,*,#6220,.T.) ;
#8757 = ORIENTED_EDGE('',*,*,#6231,.T.) ;
#8758 = ORIENTED_EDGE('',*,*,#6228,.T.) ;
#8759 = ORIENTED_EDGE('',*,*,#6225,.T.) ;
#8760 = ORIENTED_EDGE('',*,*,#6216,.T.) ;
#8761 = ORIENTED_EDGE('',*,*,#6233,.F.) ;
#8762 = ORIENTED_EDGE('',*,*,#6234,.F.) ;
#8763 = ORIENTED_EDGE('',*,*,#6221,.T.) ;
#8764 = ORIENTED_EDGE('',*,*,#6218,.F.) ;
#8765 = ORIENTED_EDGE('',*,*,#6224,.F.) ;
#8766 = ORIENTED_EDGE('',*,*,#6227,.F.) ;
#8767 = ORIENTED_EDGE('',*,*,#6230,.F.) ;
#8768 = ORIENTED_EDGE('',*,*,#6223,.F.) ;
#8769 = ORIENTED_EDGE('',*,*,#6234,.T.) ;
#8770 = ORIENTED_EDGE('',*,*,#6235,.F.) ;
#8771 = ORIENTED_EDGE('',*,*,#6236,.F.) ;
#8772 = ORIENTED_EDGE('',*,*,#6237,.T.) ;
#8773 = ORIENTED_EDGE('',*,*,#6238,.F.) ;
#8774 = ORIENTED_EDGE('',*,*,#6239,.F.) ;
#8775 = ORIENTED_EDGE('',*,*,#6237,.F.) ;
#8776 = ORIENTED_EDGE('',*,*,#6240,.F.) ;
#8777 = ORIENTED_EDGE('',*,*,#6241,.F.) ;
#8778 = ORIENTED_EDGE('',*,*,#6242,.F.) ;
#8779 = ORIENTED_EDGE('',*,*,#6243,.F.) ;
#8780 = ORIENTED_EDGE('',*,*,#6244,.F.) ;
#8781 = ORIENTED_EDGE('',*,*,#6245,.F.) ;
#8782 = ORIENTED_EDGE('',*,*,#6246,.F.) ;
#8783 = ORIENTED_EDGE('',*,*,#6247,.F.) ;
#8784 = ORIENTED_EDGE('',*,*,#6248,.T.) ;
#8785 = ORIENTED_EDGE('',*,*,#6246,.T.) ;
#8786 = ORIENTED_EDGE('',*,*,#6248,.F.) ;
#8787 = ORIENTED_EDGE('',*,*,#6242,.T.) ;
#8788 = ORIENTED_EDGE('',*,*,#6249,.T.) ;
#8789 = ORIENTED_EDGE('',*,*,#6250,.F.) ;
#8790 = ORIENTED_EDGE('',*,*,#6251,.F.) ;
#8791 = ORIENTED_EDGE('',*,*,#6243,.T.) ;
#8792 = ORIENTED_EDGE('',*,*,#6251,.T.) ;
#8793 = ORIENTED_EDGE('',*,*,#6252,.F.) ;
#8794 = ORIENTED_EDGE('',*,*,#6253,.F.) ;
#8795 = ORIENTED_EDGE('',*,*,#6244,.T.) ;
#8796 = ORIENTED_EDGE('',*,*,#6253,.T.) ;
#8797 = ORIENTED_EDGE('',*,*,#6254,.F.) ;
#8798 = ORIENTED_EDGE('',*,*,#6255,.F.) ;
#8799 = ORIENTED_EDGE('',*,*,#6256,.F.) ;
#8800 = ORIENTED_EDGE('',*,*,#6245,.T.) ;
#8801 = ORIENTED_EDGE('',*,*,#6255,.T.) ;
#8802 = ORIENTED_EDGE('',*,*,#6257,.F.) ;
#8803 = ORIENTED_EDGE('',*,*,#6249,.F.) ;
#8804 = ORIENTED_EDGE('',*,*,#6241,.T.) ;
#8805 = ORIENTED_EDGE('',*,*,#6257,.T.) ;
#8806 = ORIENTED_EDGE('',*,*,#6254,.T.) ;
#8807 = ORIENTED_EDGE('',*,*,#6252,.T.) ;
#8808 = ORIENTED_EDGE('',*,*,#6250,.T.) ;
#8809 = ORIENTED_EDGE('',*,*,#6247,.T.) ;
#8810 = ORIENTED_EDGE('',*,*,#6258,.F.) ;
#8811 = ORIENTED_EDGE('',*,*,#6259,.T.) ;
#8812 = ORIENTED_EDGE('',*,*,#6235,.T.) ;
#8813 = ORIENTED_EDGE('',*,*,#6233,.T.) ;
#8814 = ORIENTED_EDGE('',*,*,#6215,.T.) ;
#8815 = ORIENTED_EDGE('',*,*,#6232,.T.) ;
#8816 = ORIENTED_EDGE('',*,*,#6238,.T.) ;
#8817 = ORIENTED_EDGE('',*,*,#6239,.T.) ;
#8818 = ORIENTED_EDGE('',*,*,#6256,.T.) ;
#8819 = ORIENTED_EDGE('',*,*,#6240,.T.) ;
#8820 = ORIENTED_EDGE('',*,*,#6236,.T.) ;
#8821 = ORIENTED_EDGE('',*,*,#6259,.F.) ;
#8822 = ORIENTED_EDGE('',*,*,#6260,.T.) ;
#8823 = ORIENTED_EDGE('',*,*,#6260,.F.) ;
#8824 = ORIENTED_EDGE('',*,*,#6261,.T.) ;
#8825 = ORIENTED_EDGE('',*,*,#6262,.F.) ;
#8826 = ORIENTED_EDGE('',*,*,#6261,.F.) ;
#8827 = ORIENTED_EDGE('',*,*,#6263,.T.) ;
#8828 = ORIENTED_EDGE('',*,*,#6264,.T.) ;
#8829 = ORIENTED_EDGE('',*,*,#6265,.F.) ;
#8830 = ORIENTED_EDGE('',*,*,#6266,.F.) ;
#8831 = ORIENTED_EDGE('',*,*,#6267,.T.) ;
#8832 = ORIENTED_EDGE('',*,*,#6266,.T.) ;
#8833 = ORIENTED_EDGE('',*,*,#6268,.F.) ;
#8834 = ORIENTED_EDGE('',*,*,#6269,.F.) ;
#8835 = ORIENTED_EDGE('',*,*,#6270,.T.) ;
#8836 = ORIENTED_EDGE('',*,*,#6269,.T.) ;
#8837 = ORIENTED_EDGE('',*,*,#6271,.F.) ;
#8838 = ORIENTED_EDGE('',*,*,#6272,.F.) ;
#8839 = ORIENTED_EDGE('',*,*,#6273,.T.) ;
#8840 = ORIENTED_EDGE('',*,*,#6272,.T.) ;
#8841 = ORIENTED_EDGE('',*,*,#6274,.F.) ;
#8842 = ORIENTED_EDGE('',*,*,#6264,.F.) ;
#8843 = ORIENTED_EDGE('',*,*,#6274,.T.) ;
#8844 = ORIENTED_EDGE('',*,*,#6271,.T.) ;
#8845 = ORIENTED_EDGE('',*,*,#6268,.T.) ;
#8846 = ORIENTED_EDGE('',*,*,#6265,.T.) ;
#8847 = ORIENTED_EDGE('',*,*,#6209,.T.) ;
#8848 = ORIENTED_EDGE('',*,*,#6212,.T.) ;
#8849 = ORIENTED_EDGE('',*,*,#6262,.T.) ;
#8850 = ORIENTED_EDGE('',*,*,#6273,.F.) ;
#8851 = ORIENTED_EDGE('',*,*,#6263,.F.) ;
#8852 = ORIENTED_EDGE('',*,*,#6267,.F.) ;
#8853 = ORIENTED_EDGE('',*,*,#6270,.F.) ;
#8854 = ORIENTED_EDGE('',*,*,#6211,.T.) ;
#8855 = ORIENTED_EDGE('',*,*,#6214,.T.) ;
#8856 = ORIENTED_EDGE('',*,*,#6258,.T.) ;
#8857 = ORIENTED_EDGE('',*,*,#6275,.F.) ;
#8858 = ORIENTED_EDGE('',*,*,#6276,.T.) ;
#8859 = ORIENTED_EDGE('',*,*,#6277,.F.) ;
#8860 = ORIENTED_EDGE('',*,*,#6276,.F.) ;
#8861 = ORIENTED_EDGE('',*,*,#6278,.F.) ;
#8862 = ORIENTED_EDGE('',*,*,#6279,.T.) ;
#8863 = ORIENTED_EDGE('',*,*,#6280,.F.) ;
#8864 = ORIENTED_EDGE('',*,*,#6279,.F.) ;
#8865 = ORIENTED_EDGE('',*,*,#6281,.F.) ;
#8866 = ORIENTED_EDGE('',*,*,#6282,.T.) ;
#8867 = ORIENTED_EDGE('',*,*,#6283,.T.) ;
#8868 = ORIENTED_EDGE('',*,*,#6284,.T.) ;
#8869 = ORIENTED_EDGE('',*,*,#6285,.T.) ;
#8870 = ORIENTED_EDGE('',*,*,#6286,.F.) ;
#8871 = ORIENTED_EDGE('',*,*,#6287,.T.) ;
#8872 = ORIENTED_EDGE('',*,*,#6288,.T.) ;
#8873 = ORIENTED_EDGE('',*,*,#6282,.F.) ;
#8874 = ORIENTED_EDGE('',*,*,#6285,.F.) ;
#8875 = ORIENTED_EDGE('',*,*,#6289,.T.) ;
#8876 = ORIENTED_EDGE('',*,*,#6290,.T.) ;
#8877 = ORIENTED_EDGE('',*,*,#6289,.F.) ;
#8878 = ORIENTED_EDGE('',*,*,#6291,.F.) ;
#8879 = ORIENTED_EDGE('',*,*,#6284,.F.) ;
#8880 = ORIENTED_EDGE('',*,*,#6292,.F.) ;
#8881 = ORIENTED_EDGE('',*,*,#6293,.T.) ;
#8882 = ORIENTED_EDGE('',*,*,#6294,.T.) ;
#8883 = ORIENTED_EDGE('',*,*,#6292,.T.) ;
#8884 = ORIENTED_EDGE('',*,*,#6283,.F.) ;
#8885 = ORIENTED_EDGE('',*,*,#6288,.F.) ;
#8886 = ORIENTED_EDGE('',*,*,#6295,.F.) ;
#8887 = ORIENTED_EDGE('',*,*,#6293,.F.) ;
#8888 = ORIENTED_EDGE('',*,*,#6294,.F.) ;
#8889 = ORIENTED_EDGE('',*,*,#6287,.F.) ;
#8890 = ORIENTED_EDGE('',*,*,#6290,.F.) ;
#8891 = ORIENTED_EDGE('',*,*,#6296,.F.) ;
#8892 = ORIENTED_EDGE('',*,*,#6297,.T.) ;
#8893 = ORIENTED_EDGE('',*,*,#6298,.T.) ;
#8894 = ORIENTED_EDGE('',*,*,#6299,.T.) ;
#8895 = ORIENTED_EDGE('',*,*,#6300,.T.) ;
#8896 = ORIENTED_EDGE('',*,*,#6301,.F.) ;
#8897 = ORIENTED_EDGE('',*,*,#6302,.T.) ;
#8898 = ORIENTED_EDGE('',*,*,#6303,.T.) ;
#8899 = ORIENTED_EDGE('',*,*,#6297,.F.) ;
#8900 = ORIENTED_EDGE('',*,*,#6300,.F.) ;
#8901 = ORIENTED_EDGE('',*,*,#6304,.T.) ;
#8902 = ORIENTED_EDGE('',*,*,#6305,.T.) ;
#8903 = ORIENTED_EDGE('',*,*,#6304,.F.) ;
#8904 = ORIENTED_EDGE('',*,*,#6306,.F.) ;
#8905 = ORIENTED_EDGE('',*,*,#6299,.F.) ;
#8906 = ORIENTED_EDGE('',*,*,#6307,.F.) ;
#8907 = ORIENTED_EDGE('',*,*,#6308,.T.) ;
#8908 = ORIENTED_EDGE('',*,*,#6309,.T.) ;
#8909 = ORIENTED_EDGE('',*,*,#6307,.T.) ;
#8910 = ORIENTED_EDGE('',*,*,#6298,.F.) ;
#8911 = ORIENTED_EDGE('',*,*,#6303,.F.) ;
#8912 = ORIENTED_EDGE('',*,*,#6310,.F.) ;
#8913 = ORIENTED_EDGE('',*,*,#6308,.F.) ;
#8914 = ORIENTED_EDGE('',*,*,#6309,.F.) ;
#8915 = ORIENTED_EDGE('',*,*,#6302,.F.) ;
#8916 = ORIENTED_EDGE('',*,*,#6305,.F.) ;
#8917 = ORIENTED_EDGE('',*,*,#6311,.T.) ;
#8918 = ORIENTED_EDGE('',*,*,#6312,.T.) ;
#8919 = ORIENTED_EDGE('',*,*,#6313,.F.) ;
#8920 = ORIENTED_EDGE('',*,*,#6314,.F.) ;
#8921 = ORIENTED_EDGE('',*,*,#6315,.T.) ;
#8922 = ORIENTED_EDGE('',*,*,#6314,.T.) ;
#8923 = ORIENTED_EDGE('',*,*,#6316,.F.) ;
#8924 = ORIENTED_EDGE('',*,*,#6317,.F.) ;
#8925 = ORIENTED_EDGE('',*,*,#6318,.T.) ;
#8926 = ORIENTED_EDGE('',*,*,#6317,.T.) ;
#8927 = ORIENTED_EDGE('',*,*,#6319,.F.) ;
#8928 = ORIENTED_EDGE('',*,*,#6320,.F.) ;
#8929 = ORIENTED_EDGE('',*,*,#6321,.T.) ;
#8930 = ORIENTED_EDGE('',*,*,#6320,.T.) ;
#8931 = ORIENTED_EDGE('',*,*,#6322,.F.) ;
#8932 = ORIENTED_EDGE('',*,*,#6312,.F.) ;
#8933 = ORIENTED_EDGE('',*,*,#6322,.T.) ;
#8934 = ORIENTED_EDGE('',*,*,#6319,.T.) ;
#8935 = ORIENTED_EDGE('',*,*,#6316,.T.) ;
#8936 = ORIENTED_EDGE('',*,*,#6313,.T.) ;
#8937 = ORIENTED_EDGE('',*,*,#6275,.T.) ;
#8938 = ORIENTED_EDGE('',*,*,#6278,.T.) ;
#8939 = ORIENTED_EDGE('',*,*,#6321,.F.) ;
#8940 = ORIENTED_EDGE('',*,*,#6311,.F.) ;
#8941 = ORIENTED_EDGE('',*,*,#6315,.F.) ;
#8942 = ORIENTED_EDGE('',*,*,#6318,.F.) ;
#8943 = ORIENTED_EDGE('',*,*,#6277,.T.) ;
#8944 = ORIENTED_EDGE('',*,*,#6280,.T.) ;
#8945 = ORIENTED_EDGE('',*,*,#6286,.T.) ;
#8946 = ORIENTED_EDGE('',*,*,#6281,.T.) ;
#8947 = ORIENTED_EDGE('',*,*,#6291,.T.) ;
#8948 = ORIENTED_EDGE('',*,*,#6295,.T.) ;
#8949 = ORIENTED_EDGE('',*,*,#6301,.T.) ;
#8950 = ORIENTED_EDGE('',*,*,#6296,.T.) ;
#8951 = ORIENTED_EDGE('',*,*,#6306,.T.) ;
#8952 = ORIENTED_EDGE('',*,*,#6310,.T.) ;
#8953 = ORIENTED_EDGE('',*,*,#6323,.F.) ;
#8954 = ORIENTED_EDGE('',*,*,#6324,.T.) ;
#8955 = ORIENTED_EDGE('',*,*,#6325,.F.) ;
#8956 = ORIENTED_EDGE('',*,*,#6326,.T.) ;
#8957 = ORIENTED_EDGE('',*,*,#6323,.T.) ;
#8958 = ORIENTED_EDGE('',*,*,#6326,.F.) ;
#8959 = ORIENTED_EDGE('',*,*,#6327,.F.) ;
#8960 = ORIENTED_EDGE('',*,*,#6325,.T.) ;
#8961 = ORIENTED_EDGE('',*,*,#6328,.F.) ;
#8962 = ORIENTED_EDGE('',*,*,#6329,.T.) ;
#8963 = ORIENTED_EDGE('',*,*,#6327,.T.) ;
#8964 = ORIENTED_EDGE('',*,*,#6329,.F.) ;
#8965 = ORIENTED_EDGE('',*,*,#6330,.F.) ;
#8966 = ORIENTED_EDGE('',*,*,#6331,.T.) ;
#8967 = ORIENTED_EDGE('',*,*,#6328,.T.) ;
#8968 = ORIENTED_EDGE('',*,*,#6331,.F.) ;
#8969 = ORIENTED_EDGE('',*,*,#6332,.F.) ;
#8970 = ORIENTED_EDGE('',*,*,#6333,.T.) ;
#8971 = ORIENTED_EDGE('',*,*,#6330,.T.) ;
#8972 = ORIENTED_EDGE('',*,*,#6333,.F.) ;
#8973 = ORIENTED_EDGE('',*,*,#6334,.F.) ;
#8974 = ORIENTED_EDGE('',*,*,#6335,.T.) ;
#8975 = ORIENTED_EDGE('',*,*,#6332,.T.) ;
#8976 = ORIENTED_EDGE('',*,*,#6335,.F.) ;
#8977 = ORIENTED_EDGE('',*,*,#6336,.F.) ;
#8978 = ORIENTED_EDGE('',*,*,#6337,.T.) ;
#8979 = ORIENTED_EDGE('',*,*,#6334,.T.) ;
#8980 = ORIENTED_EDGE('',*,*,#6337,.F.) ;
#8981 = ORIENTED_EDGE('',*,*,#6336,.T.) ;
#8982 = ORIENTED_EDGE('',*,*,#6338,.F.) ;
#8983 = ORIENTED_EDGE('',*,*,#6339,.F.) ;
#8984 = ORIENTED_EDGE('',*,*,#6340,.T.) ;
#8985 = ORIENTED_EDGE('',*,*,#6338,.T.) ;
#8986 = ORIENTED_EDGE('',*,*,#6340,.F.) ;
#8987 = ORIENTED_EDGE('',*,*,#6339,.T.) ;
#8988 = ORIENTED_EDGE('',*,*,#6341,.F.) ;
#8989 = ORIENTED_EDGE('',*,*,#6341,.T.) ;
#8990 = ORIENTED_EDGE('',*,*,#6342,.T.) ;
#8991 = ORIENTED_EDGE('',*,*,#6324,.F.) ;
#8992 = ORIENTED_EDGE('',*,*,#6342,.F.) ;
#8993 = CONICAL_SURFACE('',#9749,1.12500000000001,0.785398163397463) ;
#8994 = CONICAL_SURFACE('',#9756,1.12500000000001,0.785398163397463) ;
#8995 = CONICAL_SURFACE('',#9763,1.12500000000001,0.785398163397463) ;
#8996 = CONICAL_SURFACE('',#9770,1.12500000000001,0.785398163397463) ;
#8997 = CONICAL_SURFACE('',#9777,1.125,0.785398163397434) ;
#8998 = CONICAL_SURFACE('',#9782,1.125,0.785398163397434) ;
#8999 = CONICAL_SURFACE('',#9787,1.125,0.785398163397434) ;
#9000 = CONICAL_SURFACE('',#9791,1.125,0.785398163397434) ;
#9001 = CONICAL_SURFACE('',#9795,1.04999999999999,1.02974425867665) ;
#9002 = CONICAL_SURFACE('',#9796,1.05,1.02974425867665) ;
#9003 = CONICAL_SURFACE('',#9797,1.04999999999999,1.02974425867665) ;
#9004 = CONICAL_SURFACE('',#9798,1.05,1.02974425867665) ;
#9005 = CONICAL_SURFACE('',#9799,1.05,1.02974425867665) ;
#9006 = CONICAL_SURFACE('',#9803,1.05,1.02974425867666) ;
#9007 = CONICAL_SURFACE('',#9804,1.05,1.02974425867665) ;
#9008 = CONICAL_SURFACE('',#9808,1.05,1.02974425867666) ;
#9009 = CONICAL_SURFACE('',#10138,4.75,0.785398163397457) ;
#9010 = CONICAL_SURFACE('',#10222,2.9,0.78539816339747) ;
#9011 = CONICAL_SURFACE('',#10238,1.875,0.785398163397448) ;
#9012 = CONICAL_SURFACE('',#10257,3.85000000000001,0.785398163397434) ;
#9013 = CONICAL_SURFACE('',#10261,3.85000000000001,0.785398163397448) ;
#9014 = CONICAL_SURFACE('',#10267,1.40000000000001,0.785398163397448) ;
#9015 = CONICAL_SURFACE('',#10316,0.791749999999999,0.785398163397448) ;
#9016 = CONICAL_SURFACE('',#10400,1.75,0.785398163397441) ;
#9017 = CONICAL_SURFACE('',#10508,0.916025403784442,0.785398163397437) ;
#9018 = CONICAL_SURFACE('',#10548,0.866025403784434,1.02974425867665) ;
#9019 = CONICAL_SURFACE('',#10640,10.35,1.16590454050981) ;
#9020 = CONICAL_SURFACE('',#10642,11.35,0.828849058788986) ;
#9021 = CONICAL_SURFACE('',#10646,11.35,0.828849058788986) ;
#9022 = CONICAL_SURFACE('',#10648,10.35,1.16590454050981) ;
#9023 = ADVANCED_FACE('',(#1087),#8993,.F.) ;
#9024 = ADVANCED_FACE('',(#1088,#651,#652),#759,.F.) ;
#9025 = ADVANCED_FACE('',(#1089),#500,.F.) ;
#9026 = ADVANCED_FACE('',(#1090),#8994,.F.) ;
#9027 = ADVANCED_FACE('',(#1091,#653,#654),#760,.F.) ;
#9028 = ADVANCED_FACE('',(#1092),#501,.F.) ;
#9029 = ADVANCED_FACE('',(#1093),#8995,.F.) ;
#9030 = ADVANCED_FACE('',(#1094,#655,#656),#761,.F.) ;
#9031 = ADVANCED_FACE('',(#1095),#502,.F.) ;
#9032 = ADVANCED_FACE('',(#1096),#8996,.F.) ;
#9033 = ADVANCED_FACE('',(#1097,#657,#658),#762,.F.) ;
#9034 = ADVANCED_FACE('',(#1098),#503,.F.) ;
#9035 = ADVANCED_FACE('',(#1099),#8997,.F.) ;
#9036 = ADVANCED_FACE('',(#1100),#504,.F.) ;
#9037 = ADVANCED_FACE('',(#1101),#8998,.F.) ;
#9038 = ADVANCED_FACE('',(#1102),#505,.F.) ;
#9039 = ADVANCED_FACE('',(#1103),#8999,.F.) ;
#9040 = ADVANCED_FACE('',(#1104),#506,.F.) ;
#9041 = ADVANCED_FACE('',(#1105),#9000,.F.) ;
#9042 = ADVANCED_FACE('',(#1106),#507,.F.) ;
#9043 = ADVANCED_FACE('',(#1107),#9001,.F.) ;
#9044 = ADVANCED_FACE('',(#1108),#9002,.F.) ;
#9045 = ADVANCED_FACE('',(#1109),#9003,.F.) ;
#9046 = ADVANCED_FACE('',(#1110),#9004,.F.) ;
#9047 = ADVANCED_FACE('',(#1111),#9005,.F.) ;
#9048 = ADVANCED_FACE('',(#1112,#659),#508,.F.) ;
#9049 = ADVANCED_FACE('',(#1113),#9006,.F.) ;
#9050 = ADVANCED_FACE('',(#1114),#9007,.F.) ;
#9051 = ADVANCED_FACE('',(#1115,#660),#509,.F.) ;
#9052 = ADVANCED_FACE('',(#1116),#9008,.F.) ;
#9053 = ADVANCED_FACE('',(#1117),#510,.F.) ;
#9054 = ADVANCED_FACE('',(#1118,#661),#511,.F.) ;
#9055 = ADVANCED_FACE('',(#1119),#763,.T.) ;
#9056 = ADVANCED_FACE('',(#1120),#512,.F.) ;
#9057 = ADVANCED_FACE('',(#1121,#662),#513,.F.) ;
#9058 = ADVANCED_FACE('',(#1122),#764,.T.) ;
#9059 = ADVANCED_FACE('',(#1123),#514,.F.) ;
#9060 = ADVANCED_FACE('',(#1124),#515,.F.) ;
#9061 = ADVANCED_FACE('',(#1125),#516,.F.) ;
#9062 = ADVANCED_FACE('',(#1126),#517,.F.) ;
#9063 = ADVANCED_FACE('',(#1127),#765,.T.) ;
#9064 = ADVANCED_FACE('',(#1128,#663),#766,.T.) ;
#9065 = ADVANCED_FACE('',(#1129),#767,.T.) ;
#9066 = ADVANCED_FACE('',(#1130,#664),#768,.T.) ;
#9067 = ADVANCED_FACE('',(#1131),#769,.T.) ;
#9068 = ADVANCED_FACE('',(#1132,#665),#770,.T.) ;
#9069 = ADVANCED_FACE('',(#1133),#771,.T.) ;
#9070 = ADVANCED_FACE('',(#1134),#772,.T.) ;
#9071 = ADVANCED_FACE('',(#1135,#666),#773,.T.) ;
#9072 = ADVANCED_FACE('',(#1136,#667),#518,.T.) ;
#9073 = ADVANCED_FACE('',(#1137),#774,.T.) ;
#9074 = ADVANCED_FACE('',(#1138),#775,.T.) ;
#9075 = ADVANCED_FACE('',(#1139,#668),#776,.T.) ;
#9076 = ADVANCED_FACE('',(#1140,#669,#670),#777,.T.) ;
#9077 = ADVANCED_FACE('',(#1141),#778,.T.) ;
#9078 = ADVANCED_FACE('',(#1142),#779,.T.) ;
#9079 = ADVANCED_FACE('',(#1143),#780,.T.) ;
#9080 = ADVANCED_FACE('',(#1144),#519,.T.) ;
#9081 = ADVANCED_FACE('',(#1145,#671),#781,.F.) ;
#9082 = ADVANCED_FACE('',(#1146),#782,.T.) ;
#9083 = ADVANCED_FACE('',(#1147),#783,.T.) ;
#9084 = ADVANCED_FACE('',(#1148),#784,.T.) ;
#9085 = ADVANCED_FACE('',(#1149,#672),#520,.T.) ;
#9086 = ADVANCED_FACE('',(#1150),#785,.T.) ;
#9087 = ADVANCED_FACE('',(#1151),#786,.T.) ;
#9088 = ADVANCED_FACE('',(#1152,#673),#787,.T.) ;
#9089 = ADVANCED_FACE('',(#1153),#788,.T.) ;
#9090 = ADVANCED_FACE('',(#1154),#789,.T.) ;
#9091 = ADVANCED_FACE('',(#1155),#521,.T.) ;
#9092 = ADVANCED_FACE('',(#1156,#674),#790,.F.) ;
#9093 = ADVANCED_FACE('',(#1157),#791,.T.) ;
#9094 = ADVANCED_FACE('',(#1158),#792,.T.) ;
#9095 = ADVANCED_FACE('',(#1159),#793,.T.) ;
#9096 = ADVANCED_FACE('',(#1160),#794,.T.) ;
#9097 = ADVANCED_FACE('',(#1161),#795,.T.) ;
#9098 = ADVANCED_FACE('',(#1162),#796,.T.) ;
#9099 = ADVANCED_FACE('',(#1163),#797,.T.) ;
#9100 = ADVANCED_FACE('',(#1164),#798,.T.) ;
#9101 = ADVANCED_FACE('',(#1165),#799,.T.) ;
#9102 = ADVANCED_FACE('',(#1166),#800,.T.) ;
#9103 = ADVANCED_FACE('',(#1167),#801,.T.) ;
#9104 = ADVANCED_FACE('',(#1168),#802,.F.) ;
#9105 = ADVANCED_FACE('',(#1169),#803,.T.) ;
#9106 = ADVANCED_FACE('',(#1170,#675),#804,.T.) ;
#9107 = ADVANCED_FACE('',(#1171),#805,.T.) ;
#9108 = ADVANCED_FACE('',(#1172),#806,.T.) ;
#9109 = ADVANCED_FACE('',(#1173),#807,.T.) ;
#9110 = ADVANCED_FACE('',(#1174),#808,.T.) ;
#9111 = ADVANCED_FACE('',(#1175),#809,.T.) ;
#9112 = ADVANCED_FACE('',(#1176),#810,.F.) ;
#9113 = ADVANCED_FACE('',(#1177),#811,.T.) ;
#9114 = ADVANCED_FACE('',(#1178),#812,.T.) ;
#9115 = ADVANCED_FACE('',(#1179),#813,.T.) ;
#9116 = ADVANCED_FACE('',(#1180),#814,.T.) ;
#9117 = ADVANCED_FACE('',(#1181),#815,.T.) ;
#9118 = ADVANCED_FACE('',(#1182,#676),#816,.T.) ;
#9119 = ADVANCED_FACE('',(#1183),#817,.T.) ;
#9120 = ADVANCED_FACE('',(#1184),#818,.T.) ;
#9121 = ADVANCED_FACE('',(#1185),#522,.F.) ;
#9122 = ADVANCED_FACE('',(#1186),#523,.F.) ;
#9123 = ADVANCED_FACE('',(#1187,#677),#819,.T.) ;
#9124 = ADVANCED_FACE('',(#1188),#820,.T.) ;
#9125 = ADVANCED_FACE('',(#1189),#821,.T.) ;
#9126 = ADVANCED_FACE('',(#1190),#822,.T.) ;
#9127 = ADVANCED_FACE('',(#1191,#678),#823,.F.) ;
#9128 = ADVANCED_FACE('',(#1192),#524,.F.) ;
#9129 = ADVANCED_FACE('',(#1193),#525,.F.) ;
#9130 = ADVANCED_FACE('',(#1194,#679),#824,.F.) ;
#9131 = ADVANCED_FACE('',(#1195,#680),#825,.F.) ;
#9132 = ADVANCED_FACE('',(#1196),#826,.T.) ;
#9133 = ADVANCED_FACE('',(#1197,#681),#827,.T.) ;
#9134 = ADVANCED_FACE('',(#1198),#828,.T.) ;
#9135 = ADVANCED_FACE('',(#1199),#829,.T.) ;
#9136 = ADVANCED_FACE('',(#1200),#526,.F.) ;
#9137 = ADVANCED_FACE('',(#1201),#527,.F.) ;
#9138 = ADVANCED_FACE('',(#1202),#528,.T.) ;
#9139 = ADVANCED_FACE('',(#1203),#331,.T.) ;
#9140 = ADVANCED_FACE('',(#1204),#529,.T.) ;
#9141 = ADVANCED_FACE('',(#1205),#332,.T.) ;
#9142 = ADVANCED_FACE('',(#1206),#530,.T.) ;
#9143 = ADVANCED_FACE('',(#1207),#333,.T.) ;
#9144 = ADVANCED_FACE('',(#1208),#531,.T.) ;
#9145 = ADVANCED_FACE('',(#1209),#334,.T.) ;
#9146 = ADVANCED_FACE('',(#1210),#532,.T.) ;
#9147 = ADVANCED_FACE('',(#1211),#830,.T.) ;
#9148 = ADVANCED_FACE('',(#1212),#533,.T.) ;
#9149 = ADVANCED_FACE('',(#1213),#831,.T.) ;
#9150 = ADVANCED_FACE('',(#1214),#832,.T.) ;
#9151 = ADVANCED_FACE('',(#1215),#833,.F.) ;
#9152 = ADVANCED_FACE('',(#1216),#534,.F.) ;
#9153 = ADVANCED_FACE('',(#1217),#834,.F.) ;
#9154 = ADVANCED_FACE('',(#1218),#835,.F.) ;
#9155 = ADVANCED_FACE('',(#1219),#836,.F.) ;
#9156 = ADVANCED_FACE('',(#1220),#535,.F.) ;
#9157 = ADVANCED_FACE('',(#1221),#837,.F.) ;
#9158 = ADVANCED_FACE('',(#1222),#536,.T.) ;
#9159 = ADVANCED_FACE('',(#1223),#838,.T.) ;
#9160 = ADVANCED_FACE('',(#1224),#537,.T.) ;
#9161 = ADVANCED_FACE('',(#1225),#839,.T.) ;
#9162 = ADVANCED_FACE('',(#1226),#538,.T.) ;
#9163 = ADVANCED_FACE('',(#1227),#539,.F.) ;
#9164 = ADVANCED_FACE('',(#1228),#540,.F.) ;
#9165 = ADVANCED_FACE('',(#1229),#541,.F.) ;
#9166 = ADVANCED_FACE('',(#1230),#840,.T.) ;
#9167 = ADVANCED_FACE('',(#1231),#542,.T.) ;
#9168 = ADVANCED_FACE('',(#1232),#841,.T.) ;
#9169 = ADVANCED_FACE('',(#1233),#543,.T.) ;
#9170 = ADVANCED_FACE('',(#1234,#682,#683,#684,#685),#842,.T.) ;
#9171 = ADVANCED_FACE('',(#1235,#686,#687,#688),#843,.F.) ;
#9172 = ADVANCED_FACE('',(#1236),#544,.F.) ;
#9173 = ADVANCED_FACE('',(#1237),#545,.F.) ;
#9174 = ADVANCED_FACE('',(#1238),#546,.F.) ;
#9175 = ADVANCED_FACE('',(#1239),#844,.T.) ;
#9176 = ADVANCED_FACE('',(#1240),#547,.T.) ;
#9177 = ADVANCED_FACE('',(#1241),#845,.T.) ;
#9178 = ADVANCED_FACE('',(#1242),#548,.T.) ;
#9179 = ADVANCED_FACE('',(#1243,#689,#690,#691),#846,.T.) ;
#9180 = ADVANCED_FACE('',(#1244,#692,#693,#694,#695),#847,.F.) ;
#9181 = ADVANCED_FACE('',(#1245),#549,.T.) ;
#9182 = ADVANCED_FACE('',(#1246),#550,.T.) ;
#9183 = ADVANCED_FACE('',(#1247),#551,.F.) ;
#9184 = ADVANCED_FACE('',(#1248),#552,.F.) ;
#9185 = ADVANCED_FACE('',(#1249),#553,.F.) ;
#9186 = ADVANCED_FACE('',(#1250),#848,.T.) ;
#9187 = ADVANCED_FACE('',(#1251),#554,.T.) ;
#9188 = ADVANCED_FACE('',(#1252),#849,.T.) ;
#9189 = ADVANCED_FACE('',(#1253),#555,.T.) ;
#9190 = ADVANCED_FACE('',(#1254,#696,#697,#698,#699,#700),#850,.T.) ;
#9191 = ADVANCED_FACE('',(#1255,#701,#702,#703),#851,.F.) ;
#9192 = ADVANCED_FACE('',(#1256),#556,.F.) ;
#9193 = ADVANCED_FACE('',(#1257),#557,.F.) ;
#9194 = ADVANCED_FACE('',(#1258),#558,.F.) ;
#9195 = ADVANCED_FACE('',(#1259),#852,.T.) ;
#9196 = ADVANCED_FACE('',(#1260),#559,.T.) ;
#9197 = ADVANCED_FACE('',(#1261),#853,.T.) ;
#9198 = ADVANCED_FACE('',(#1262),#560,.T.) ;
#9199 = ADVANCED_FACE('',(#1263,#704,#705,#706),#854,.T.) ;
#9200 = ADVANCED_FACE('',(#1264,#707,#708,#709,#710,#711),#855,.F.) ;
#9201 = ADVANCED_FACE('',(#1265),#561,.T.) ;
#9202 = ADVANCED_FACE('',(#1266),#562,.T.) ;
#9203 = ADVANCED_FACE('',(#1267),#563,.F.) ;
#9204 = ADVANCED_FACE('',(#1268),#856,.T.) ;
#9205 = ADVANCED_FACE('',(#1269),#564,.F.) ;
#9206 = ADVANCED_FACE('',(#1270,#712),#857,.T.) ;
#9207 = ADVANCED_FACE('',(#1271),#565,.F.) ;
#9208 = ADVANCED_FACE('',(#1272,#713),#858,.T.) ;
#9209 = ADVANCED_FACE('',(#1273),#566,.T.) ;
#9210 = ADVANCED_FACE('',(#1274,#714),#859,.T.) ;
#9211 = ADVANCED_FACE('',(#1275),#567,.T.) ;
#9212 = ADVANCED_FACE('',(#1276),#568,.T.) ;
#9213 = ADVANCED_FACE('',(#1277,#715),#860,.T.) ;
#9214 = ADVANCED_FACE('',(#1278,#716),#861,.F.) ;
#9215 = ADVANCED_FACE('',(#1279),#569,.T.) ;
#9216 = ADVANCED_FACE('',(#1280),#570,.F.) ;
#9217 = ADVANCED_FACE('',(#1281),#571,.T.) ;
#9218 = ADVANCED_FACE('',(#1282,#717),#862,.T.) ;
#9219 = ADVANCED_FACE('',(#1283,#718),#863,.F.) ;
#9220 = ADVANCED_FACE('',(#1284),#864,.T.) ;
#9221 = ADVANCED_FACE('',(#1285),#865,.T.) ;
#9222 = ADVANCED_FACE('',(#1286),#572,.T.) ;
#9223 = ADVANCED_FACE('',(#1287,#719),#866,.T.) ;
#9224 = ADVANCED_FACE('',(#1288),#573,.T.) ;
#9225 = ADVANCED_FACE('',(#1289),#867,.T.) ;
#9226 = ADVANCED_FACE('',(#1290),#574,.F.) ;
#9227 = ADVANCED_FACE('',(#1291),#868,.F.) ;
#9228 = ADVANCED_FACE('',(#1292),#869,.T.) ;
#9229 = ADVANCED_FACE('',(#1293),#870,.T.) ;
#9230 = ADVANCED_FACE('',(#1294),#871,.T.) ;
#9231 = ADVANCED_FACE('',(#1295),#872,.T.) ;
#9232 = ADVANCED_FACE('',(#1296),#873,.T.) ;
#9233 = ADVANCED_FACE('',(#1297),#874,.T.) ;
#9234 = ADVANCED_FACE('',(#1298),#875,.T.) ;
#9235 = ADVANCED_FACE('',(#1299),#876,.T.) ;
#9236 = ADVANCED_FACE('',(#1300),#9009,.T.) ;
#9237 = ADVANCED_FACE('',(#1301),#877,.T.) ;
#9238 = ADVANCED_FACE('',(#1302),#575,.T.) ;
#9239 = ADVANCED_FACE('',(#1303),#878,.T.) ;
#9240 = ADVANCED_FACE('',(#1304),#879,.T.) ;
#9241 = ADVANCED_FACE('',(#1305),#880,.T.) ;
#9242 = ADVANCED_FACE('',(#1306),#881,.T.) ;
#9243 = ADVANCED_FACE('',(#1307),#882,.T.) ;
#9244 = ADVANCED_FACE('',(#1308),#883,.F.) ;
#9245 = ADVANCED_FACE('',(#1309),#884,.T.) ;
#9246 = ADVANCED_FACE('',(#1310),#885,.T.) ;
#9247 = ADVANCED_FACE('',(#1311),#886,.T.) ;
#9248 = ADVANCED_FACE('',(#1312),#887,.T.) ;
#9249 = ADVANCED_FACE('',(#1313),#888,.F.) ;
#9250 = ADVANCED_FACE('',(#1314,#720),#889,.T.) ;
#9251 = ADVANCED_FACE('',(#1315),#890,.T.) ;
#9252 = ADVANCED_FACE('',(#1316),#576,.F.) ;
#9253 = ADVANCED_FACE('',(#1317),#577,.T.) ;
#9254 = ADVANCED_FACE('',(#1318),#891,.T.) ;
#9255 = ADVANCED_FACE('',(#1319),#578,.T.) ;
#9256 = ADVANCED_FACE('',(#1320,#721),#892,.F.) ;
#9257 = ADVANCED_FACE('',(#1321),#579,.F.) ;
#9258 = ADVANCED_FACE('',(#1322),#580,.F.) ;
#9259 = ADVANCED_FACE('',(#1323),#581,.F.) ;
#9260 = ADVANCED_FACE('',(#1324),#893,.T.) ;
#9261 = ADVANCED_FACE('',(#1325),#894,.T.) ;
#9262 = ADVANCED_FACE('',(#1326,#722),#895,.T.) ;
#9263 = ADVANCED_FACE('',(#1327),#896,.T.) ;
#9264 = ADVANCED_FACE('',(#1328,#723),#897,.T.) ;
#9265 = ADVANCED_FACE('',(#1329),#898,.T.) ;
#9266 = ADVANCED_FACE('',(#1330),#899,.F.) ;
#9267 = ADVANCED_FACE('',(#1331,#724),#582,.T.) ;
#9268 = ADVANCED_FACE('',(#1332),#335,.T.) ;
#9269 = ADVANCED_FACE('',(#1333),#583,.T.) ;
#9270 = ADVANCED_FACE('',(#1334),#336,.T.) ;
#9271 = ADVANCED_FACE('',(#1335,#725,#726),#584,.T.) ;
#9272 = ADVANCED_FACE('',(#1336),#900,.T.) ;
#9273 = ADVANCED_FACE('',(#1337),#901,.F.) ;
#9274 = ADVANCED_FACE('',(#1338),#585,.F.) ;
#9275 = ADVANCED_FACE('',(#1339),#902,.T.) ;
#9276 = ADVANCED_FACE('',(#1340),#586,.T.) ;
#9277 = ADVANCED_FACE('',(#1341),#903,.T.) ;
#9278 = ADVANCED_FACE('',(#1342),#587,.T.) ;
#9279 = ADVANCED_FACE('',(#1343,#727),#904,.T.) ;
#9280 = ADVANCED_FACE('',(#1344,#728),#905,.F.) ;
#9281 = ADVANCED_FACE('',(#1345),#906,.T.) ;
#9282 = ADVANCED_FACE('',(#1346),#9010,.T.) ;
#9283 = ADVANCED_FACE('',(#1347),#588,.T.) ;
#9284 = ADVANCED_FACE('',(#1348,#729),#907,.T.) ;
#9285 = ADVANCED_FACE('',(#1349),#589,.T.) ;
#9286 = ADVANCED_FACE('',(#1350,#730),#908,.T.) ;
#9287 = ADVANCED_FACE('',(#1351),#590,.T.) ;
#9288 = ADVANCED_FACE('',(#1352,#731),#909,.T.) ;
#9289 = ADVANCED_FACE('',(#1353),#591,.T.) ;
#9290 = ADVANCED_FACE('',(#1354),#9011,.T.) ;
#9291 = ADVANCED_FACE('',(#1355),#910,.T.) ;
#9292 = ADVANCED_FACE('',(#1356),#911,.F.) ;
#9293 = ADVANCED_FACE('',(#1357),#912,.F.) ;
#9294 = ADVANCED_FACE('',(#1358),#913,.F.) ;
#9295 = ADVANCED_FACE('',(#1359),#914,.F.) ;
#9296 = ADVANCED_FACE('',(#1360),#592,.F.) ;
#9297 = ADVANCED_FACE('',(#1361),#915,.T.) ;
#9298 = ADVANCED_FACE('',(#1362),#593,.T.) ;
#9299 = ADVANCED_FACE('',(#1363),#916,.T.) ;
#9300 = ADVANCED_FACE('',(#1364),#917,.T.) ;
#9301 = ADVANCED_FACE('',(#1365),#9012,.T.) ;
#9302 = ADVANCED_FACE('',(#1366),#594,.T.) ;
#9303 = ADVANCED_FACE('',(#1367),#9013,.T.) ;
#9304 = ADVANCED_FACE('',(#1368,#732),#918,.T.) ;
#9305 = ADVANCED_FACE('',(#1369),#595,.T.) ;
#9306 = ADVANCED_FACE('',(#1370),#9014,.T.) ;
#9307 = ADVANCED_FACE('',(#1371),#919,.T.) ;
#9308 = ADVANCED_FACE('',(#1372),#596,.T.) ;
#9309 = ADVANCED_FACE('',(#1373),#597,.T.) ;
#9310 = ADVANCED_FACE('',(#1374),#598,.T.) ;
#9311 = ADVANCED_FACE('',(#1375),#599,.T.) ;
#9312 = ADVANCED_FACE('',(#1376),#600,.T.) ;
#9313 = ADVANCED_FACE('',(#1377),#601,.T.) ;
#9314 = ADVANCED_FACE('',(#1378),#602,.T.) ;
#9315 = ADVANCED_FACE('',(#1379),#603,.T.) ;
#9316 = ADVANCED_FACE('',(#1380),#604,.T.) ;
#9317 = ADVANCED_FACE('',(#1381),#605,.T.) ;
#9318 = ADVANCED_FACE('',(#1382),#606,.T.) ;
#9319 = ADVANCED_FACE('',(#1383),#607,.T.) ;
#9320 = ADVANCED_FACE('',(#1384),#608,.T.) ;
#9321 = ADVANCED_FACE('',(#1385),#609,.T.) ;
#9322 = ADVANCED_FACE('',(#1386),#610,.T.) ;
#9323 = ADVANCED_FACE('',(#1387),#611,.T.) ;
#9324 = ADVANCED_FACE('',(#1388),#612,.T.) ;
#9325 = ADVANCED_FACE('',(#1389),#613,.T.) ;
#9326 = ADVANCED_FACE('',(#1390),#614,.T.) ;
#9327 = ADVANCED_FACE('',(#1391),#615,.T.) ;
#9328 = ADVANCED_FACE('',(#1392),#616,.T.) ;
#9329 = ADVANCED_FACE('',(#1393),#617,.T.) ;
#9330 = ADVANCED_FACE('',(#1394),#618,.T.) ;
#9331 = ADVANCED_FACE('',(#1395),#619,.T.) ;
#9332 = ADVANCED_FACE('',(#1396),#620,.T.) ;
#9333 = ADVANCED_FACE('',(#1397),#621,.T.) ;
#9334 = ADVANCED_FACE('',(#1398),#622,.T.) ;
#9335 = ADVANCED_FACE('',(#1399),#623,.T.) ;
#9336 = ADVANCED_FACE('',(#1400),#920,.F.) ;
#9337 = ADVANCED_FACE('',(#1401),#243,.F.) ;
#9338 = ADVANCED_FACE('',(#1402),#921,.T.) ;
#9339 = ADVANCED_FACE('',(#1403),#624,.T.) ;
#9340 = ADVANCED_FACE('',(#1404),#244,.F.) ;
#9341 = ADVANCED_FACE('',(#1405),#337,.F.) ;
#9342 = ADVANCED_FACE('',(#1406),#625,.T.) ;
#9343 = ADVANCED_FACE('',(#1407,#733),#922,.T.) ;
#9344 = ADVANCED_FACE('',(#1408),#9015,.T.) ;
#9345 = ADVANCED_FACE('',(#1409),#923,.T.) ;
#9346 = ADVANCED_FACE('',(#1410),#924,.F.) ;
#9347 = ADVANCED_FACE('',(#1411),#925,.F.) ;
#9348 = ADVANCED_FACE('',(#1412),#926,.F.) ;
#9349 = ADVANCED_FACE('',(#1413),#626,.T.) ;
#9350 = ADVANCED_FACE('',(#1414),#927,.F.) ;
#9351 = ADVANCED_FACE('',(#1415),#928,.F.) ;
#9352 = ADVANCED_FACE('',(#1416),#929,.F.) ;
#9353 = ADVANCED_FACE('',(#1417),#9016,.T.) ;
#9354 = ADVANCED_FACE('',(#1418),#930,.F.) ;
#9355 = ADVANCED_FACE('',(#1419),#931,.F.) ;
#9356 = ADVANCED_FACE('',(#1420),#932,.F.) ;
#9357 = ADVANCED_FACE('',(#1421),#933,.F.) ;
#9358 = ADVANCED_FACE('',(#1422),#934,.F.) ;
#9359 = ADVANCED_FACE('',(#1423),#935,.F.) ;
#9360 = ADVANCED_FACE('',(#1424),#936,.F.) ;
#9361 = ADVANCED_FACE('',(#1425),#937,.F.) ;
#9362 = ADVANCED_FACE('',(#1426),#938,.F.) ;
#9363 = ADVANCED_FACE('',(#1427),#939,.F.) ;
#9364 = ADVANCED_FACE('',(#1428),#940,.F.) ;
#9365 = ADVANCED_FACE('',(#1429),#941,.F.) ;
#9366 = ADVANCED_FACE('',(#1430),#942,.F.) ;
#9367 = ADVANCED_FACE('',(#1431),#943,.F.) ;
#9368 = ADVANCED_FACE('',(#1432),#944,.F.) ;
#9369 = ADVANCED_FACE('',(#1433),#945,.F.) ;
#9370 = ADVANCED_FACE('',(#1434),#946,.F.) ;
#9371 = ADVANCED_FACE('',(#1435),#947,.F.) ;
#9372 = ADVANCED_FACE('',(#1436),#948,.F.) ;
#9373 = ADVANCED_FACE('',(#1437),#949,.F.) ;
#9374 = ADVANCED_FACE('',(#1438),#950,.F.) ;
#9375 = ADVANCED_FACE('',(#1439),#951,.F.) ;
#9376 = ADVANCED_FACE('',(#1440),#952,.F.) ;
#9377 = ADVANCED_FACE('',(#1441),#953,.F.) ;
#9378 = ADVANCED_FACE('',(#1442),#954,.F.) ;
#9379 = ADVANCED_FACE('',(#1443),#955,.F.) ;
#9380 = ADVANCED_FACE('',(#1444),#956,.F.) ;
#9381 = ADVANCED_FACE('',(#1445),#957,.F.) ;
#9382 = ADVANCED_FACE('',(#1446),#958,.F.) ;
#9383 = ADVANCED_FACE('',(#1447),#959,.F.) ;
#9384 = ADVANCED_FACE('',(#1448),#960,.F.) ;
#9385 = ADVANCED_FACE('',(#1449),#961,.F.) ;
#9386 = ADVANCED_FACE('',(#1450),#962,.F.) ;
#9387 = ADVANCED_FACE('',(#1451),#963,.F.) ;
#9388 = ADVANCED_FACE('',(#1452),#964,.F.) ;
#9389 = ADVANCED_FACE('',(#1453),#965,.F.) ;
#9390 = ADVANCED_FACE('',(#1454),#966,.F.) ;
#9391 = ADVANCED_FACE('',(#1455),#967,.F.) ;
#9392 = ADVANCED_FACE('',(#1456),#968,.F.) ;
#9393 = ADVANCED_FACE('',(#1457),#969,.F.) ;
#9394 = ADVANCED_FACE('',(#1458),#970,.F.) ;
#9395 = ADVANCED_FACE('',(#1459),#971,.F.) ;
#9396 = ADVANCED_FACE('',(#1460),#972,.F.) ;
#9397 = ADVANCED_FACE('',(#1461),#973,.F.) ;
#9398 = ADVANCED_FACE('',(#1462),#974,.F.) ;
#9399 = ADVANCED_FACE('',(#1463),#975,.F.) ;
#9400 = ADVANCED_FACE('',(#1464),#976,.F.) ;
#9401 = ADVANCED_FACE('',(#1465),#977,.F.) ;
#9402 = ADVANCED_FACE('',(#1466),#978,.F.) ;
#9403 = ADVANCED_FACE('',(#1467),#979,.F.) ;
#9404 = ADVANCED_FACE('',(#1468),#980,.F.) ;
#9405 = ADVANCED_FACE('',(#1469),#981,.F.) ;
#9406 = ADVANCED_FACE('',(#1470),#982,.F.) ;
#9407 = ADVANCED_FACE('',(#1471),#983,.F.) ;
#9408 = ADVANCED_FACE('',(#1472),#984,.F.) ;
#9409 = ADVANCED_FACE('',(#1473),#985,.F.) ;
#9410 = ADVANCED_FACE('',(#1474),#986,.F.) ;
#9411 = ADVANCED_FACE('',(#1475),#987,.F.) ;
#9412 = ADVANCED_FACE('',(#1476),#988,.F.) ;
#9413 = ADVANCED_FACE('',(#1477),#989,.F.) ;
#9414 = ADVANCED_FACE('',(#1478),#990,.F.) ;
#9415 = ADVANCED_FACE('',(#1479),#991,.F.) ;
#9416 = ADVANCED_FACE('',(#1480),#992,.F.) ;
#9417 = ADVANCED_FACE('',(#1481),#993,.F.) ;
#9418 = ADVANCED_FACE('',(#1482),#994,.F.) ;
#9419 = ADVANCED_FACE('',(#1483),#995,.F.) ;
#9420 = ADVANCED_FACE('',(#1484),#996,.F.) ;
#9421 = ADVANCED_FACE('',(#1485),#997,.F.) ;
#9422 = ADVANCED_FACE('',(#1486),#998,.F.) ;
#9423 = ADVANCED_FACE('',(#1487),#999,.F.) ;
#9424 = ADVANCED_FACE('',(#1488),#1000,.F.) ;
#9425 = ADVANCED_FACE('',(#1489),#1001,.F.) ;
#9426 = ADVANCED_FACE('',(#1490),#1002,.F.) ;
#9427 = ADVANCED_FACE('',(#1491),#1003,.F.) ;
#9428 = ADVANCED_FACE('',(#1492),#1004,.F.) ;
#9429 = ADVANCED_FACE('',(#1493),#1005,.F.) ;
#9430 = ADVANCED_FACE('',(#1494),#1006,.F.) ;
#9431 = ADVANCED_FACE('',(#1495),#1007,.F.) ;
#9432 = ADVANCED_FACE('',(#1496),#1008,.F.) ;
#9433 = ADVANCED_FACE('',(#1497),#1009,.F.) ;
#9434 = ADVANCED_FACE('',(#1498),#1010,.F.) ;
#9435 = ADVANCED_FACE('',(#1499),#1011,.F.) ;
#9436 = ADVANCED_FACE('',(#1500),#1012,.F.) ;
#9437 = ADVANCED_FACE('',(#1501),#1013,.F.) ;
#9438 = ADVANCED_FACE('',(#1502),#1014,.F.) ;
#9439 = ADVANCED_FACE('',(#1503),#1015,.F.) ;
#9440 = ADVANCED_FACE('',(#1504),#1016,.F.) ;
#9441 = ADVANCED_FACE('',(#1505),#1017,.F.) ;
#9442 = ADVANCED_FACE('',(#1506),#1018,.F.) ;
#9443 = ADVANCED_FACE('',(#1507),#1019,.F.) ;
#9444 = ADVANCED_FACE('',(#1508),#1020,.F.) ;
#9445 = ADVANCED_FACE('',(#1509),#1021,.F.) ;
#9446 = ADVANCED_FACE('',(#1510),#1022,.F.) ;
#9447 = ADVANCED_FACE('',(#1511),#1023,.F.) ;
#9448 = ADVANCED_FACE('',(#1512),#1024,.F.) ;
#9449 = ADVANCED_FACE('',(#1513),#1025,.F.) ;
#9450 = ADVANCED_FACE('',(#1514),#1026,.F.) ;
#9451 = ADVANCED_FACE('',(#1515),#1027,.F.) ;
#9452 = ADVANCED_FACE('',(#1516),#1028,.F.) ;
#9453 = ADVANCED_FACE('',(#1517),#1029,.F.) ;
#9454 = ADVANCED_FACE('',(#1518),#1030,.F.) ;
#9455 = ADVANCED_FACE('',(#1519),#1031,.F.) ;
#9456 = ADVANCED_FACE('',(#1520),#338,.T.) ;
#9457 = ADVANCED_FACE('',(#1521,#734),#1032,.F.) ;
#9458 = ADVANCED_FACE('',(#1522),#9017,.F.) ;
#9459 = ADVANCED_FACE('',(#1523),#627,.T.) ;
#9460 = ADVANCED_FACE('',(#1524),#628,.T.) ;
#9461 = ADVANCED_FACE('',(#1525),#629,.T.) ;
#9462 = ADVANCED_FACE('',(#1526),#630,.T.) ;
#9463 = ADVANCED_FACE('',(#1527),#631,.T.) ;
#9464 = ADVANCED_FACE('',(#1528),#632,.T.) ;
#9465 = ADVANCED_FACE('',(#1529),#1033,.F.) ;
#9466 = ADVANCED_FACE('',(#1530),#1034,.F.) ;
#9467 = ADVANCED_FACE('',(#1531),#1035,.F.) ;
#9468 = ADVANCED_FACE('',(#1532),#1036,.F.) ;
#9469 = ADVANCED_FACE('',(#1533),#1037,.F.) ;
#9470 = ADVANCED_FACE('',(#1534),#1038,.F.) ;
#9471 = ADVANCED_FACE('',(#1535),#1039,.F.) ;
#9472 = ADVANCED_FACE('',(#1536),#1040,.F.) ;
#9473 = ADVANCED_FACE('',(#1537),#1041,.F.) ;
#9474 = ADVANCED_FACE('',(#1538),#1042,.F.) ;
#9475 = ADVANCED_FACE('',(#1539),#1043,.F.) ;
#9476 = ADVANCED_FACE('',(#1540),#1044,.F.) ;
#9477 = ADVANCED_FACE('',(#1541),#1045,.F.) ;
#9478 = ADVANCED_FACE('',(#1542),#1046,.F.) ;
#9479 = ADVANCED_FACE('',(#1543),#1047,.F.) ;
#9480 = ADVANCED_FACE('',(#1544),#9018,.F.) ;
#9481 = ADVANCED_FACE('',(#1545),#1048,.F.) ;
#9482 = ADVANCED_FACE('',(#1546),#1049,.F.) ;
#9483 = ADVANCED_FACE('',(#1547),#1050,.F.) ;
#9484 = ADVANCED_FACE('',(#1548),#633,.F.) ;
#9485 = ADVANCED_FACE('',(#1549),#634,.F.) ;
#9486 = ADVANCED_FACE('',(#1550),#1051,.T.) ;
#9487 = ADVANCED_FACE('',(#1551),#635,.F.) ;
#9488 = ADVANCED_FACE('',(#1552),#1052,.T.) ;
#9489 = ADVANCED_FACE('',(#1553),#636,.T.) ;
#9490 = ADVANCED_FACE('',(#1554),#1053,.T.) ;
#9491 = ADVANCED_FACE('',(#1555,#735),#1054,.T.) ;
#9492 = ADVANCED_FACE('',(#1556,#736),#1055,.F.) ;
#9493 = ADVANCED_FACE('',(#1557),#1056,.T.) ;
#9494 = ADVANCED_FACE('',(#1558,#737),#1057,.F.) ;
#9495 = ADVANCED_FACE('',(#1559),#637,.F.) ;
#9496 = ADVANCED_FACE('',(#1560),#1058,.T.) ;
#9497 = ADVANCED_FACE('',(#1561),#638,.T.) ;
#9498 = ADVANCED_FACE('',(#1562),#1059,.T.) ;
#9499 = ADVANCED_FACE('',(#1563),#1060,.T.) ;
#9500 = ADVANCED_FACE('',(#1564,#738),#1061,.T.) ;
#9501 = ADVANCED_FACE('',(#1565),#639,.T.) ;
#9502 = ADVANCED_FACE('',(#1566),#1062,.F.) ;
#9503 = ADVANCED_FACE('',(#1567),#640,.F.) ;
#9504 = ADVANCED_FACE('',(#1568),#1063,.T.) ;
#9505 = ADVANCED_FACE('',(#1569),#1064,.T.) ;
#9506 = ADVANCED_FACE('',(#1570),#1065,.T.) ;
#9507 = ADVANCED_FACE('',(#1571),#1066,.T.) ;
#9508 = ADVANCED_FACE('',(#1572,#739,#740,#741),#1067,.T.) ;
#9509 = ADVANCED_FACE('',(#1573,#742,#743,#744),#1068,.F.) ;
#9510 = ADVANCED_FACE('',(#1574),#641,.F.) ;
#9511 = ADVANCED_FACE('',(#1575),#642,.F.) ;
#9512 = ADVANCED_FACE('',(#1576,#745),#1069,.T.) ;
#9513 = ADVANCED_FACE('',(#1577),#1070,.T.) ;
#9514 = ADVANCED_FACE('',(#1578),#643,.F.) ;
#9515 = ADVANCED_FACE('',(#1579),#1071,.T.) ;
#9516 = ADVANCED_FACE('',(#1580),#644,.T.) ;
#9517 = ADVANCED_FACE('',(#1581,#746),#1072,.F.) ;
#9518 = ADVANCED_FACE('',(#1582,#747),#1073,.T.) ;
#9519 = ADVANCED_FACE('',(#1583),#1074,.T.) ;
#9520 = ADVANCED_FACE('',(#1584),#645,.F.) ;
#9521 = ADVANCED_FACE('',(#1585),#1075,.T.) ;
#9522 = ADVANCED_FACE('',(#1586),#646,.T.) ;
#9523 = ADVANCED_FACE('',(#1587,#748),#1076,.F.) ;
#9524 = ADVANCED_FACE('',(#1588),#1077,.T.) ;
#9525 = ADVANCED_FACE('',(#1589),#1078,.T.) ;
#9526 = ADVANCED_FACE('',(#1590),#1079,.T.) ;
#9527 = ADVANCED_FACE('',(#1591),#1080,.T.) ;
#9528 = ADVANCED_FACE('',(#1592,#749,#750),#1081,.T.) ;
#9529 = ADVANCED_FACE('',(#1593,#751,#752,#753,#754),#1082,.F.) ;
#9530 = ADVANCED_FACE('',(#1594,#755),#1083,.T.) ;
#9531 = ADVANCED_FACE('',(#1595),#647,.T.) ;
#9532 = ADVANCED_FACE('',(#1596,#756),#1084,.T.) ;
#9533 = ADVANCED_FACE('',(#1597),#9019,.T.) ;
#9534 = ADVANCED_FACE('',(#1598),#9020,.T.) ;
#9535 = ADVANCED_FACE('',(#1599),#648,.T.) ;
#9536 = ADVANCED_FACE('',(#1600),#9021,.T.) ;
#9537 = ADVANCED_FACE('',(#1601),#9022,.T.) ;
#9538 = ADVANCED_FACE('',(#1602,#757),#1085,.T.) ;
#9539 = ADVANCED_FACE('',(#1603),#649,.T.) ;
#9540 = ADVANCED_FACE('',(#1604,#758),#1086,.T.) ;
#9541 = ADVANCED_FACE('',(#1605),#650,.F.) ;
#9542 = CLOSED_SHELL('',(#9023,#9024,#9025,#9026,#9027,#9028,#9029,#9030,
#9031,#9032,#9033,#9034,#9035,#9036,#9037,#9038,#9039,#9040,#9041,#9042,
#9043,#9044,#9045,#9046,#9047,#9048,#9049,#9050,#9051,#9052,#9053,#9054,
#9055,#9056,#9057,#9058,#9059,#9060,#9061,#9062,#9063,#9064,#9065,#9066,
#9067,#9068,#9069,#9070,#9071,#9072,#9073,#9074,#9075,#9076,#9077,#9078,
#9079,#9080,#9081,#9082,#9083,#9084,#9085,#9086,#9087,#9088,#9089,#9090,
#9091,#9092,#9093,#9094,#9095,#9096,#9097,#9098,#9099,#9100,#9101,#9102,
#9103,#9104,#9105,#9106,#9107,#9108,#9109,#9110,#9111,#9112,#9113,#9114,
#9115,#9116,#9117,#9118,#9119,#9120)) ;
#9543 = CLOSED_SHELL('',(#9121,#9122,#9123,#9124,#9125,#9126,#9127,#9128,
#9129,#9130,#9131,#9132,#9133,#9134,#9135,#9136,#9137,#9138,#9139,#9140,
#9141,#9142,#9143,#9144,#9145,#9146,#9147,#9148,#9149,#9150,#9151,#9152,
#9153,#9154,#9155,#9156,#9157,#9158,#9159,#9160,#9161)) ;
#9544 = CLOSED_SHELL('',(#9162,#9163,#9164,#9165,#9166,#9167,#9168,#9169,
#9170,#9171,#9172,#9173,#9174,#9175,#9176,#9177,#9178,#9179,#9180)) ;
#9545 = CLOSED_SHELL('',(#9181,#9182,#9183,#9184,#9185,#9186,#9187,#9188,
#9189,#9190,#9191,#9192,#9193,#9194,#9195,#9196,#9197,#9198,#9199,#9200)) ;
#9546 = CLOSED_SHELL('',(#9201,#9202,#9203,#9204,#9205,#9206,#9207,#9208,
#9209,#9210,#9211,#9212,#9213,#9214)) ;
#9547 = CLOSED_SHELL('',(#9215,#9216,#9217,#9218,#9219,#9220,#9221,#9222,
#9223,#9224,#9225)) ;
#9548 = CLOSED_SHELL('',(#9226,#9227,#9228,#9229,#9230,#9231,#9232,#9233,
#9234,#9235,#9236,#9237,#9238,#9239,#9240,#9241,#9242,#9243,#9244)) ;
#9549 = CLOSED_SHELL('',(#9245,#9246,#9247,#9248,#9249,#9250,#9251,#9252,
#9253,#9254,#9255,#9256)) ;
#9550 = CLOSED_SHELL('',(#9257,#9258,#9259,#9260,#9261,#9262,#9263,#9264,
#9265,#9266,#9267,#9268,#9269,#9270,#9271,#9272,#9273)) ;
#9551 = CLOSED_SHELL('',(#9274,#9275,#9276,#9277,#9278,#9279,#9280)) ;
#9552 = CLOSED_SHELL('',(#9281,#9282,#9283,#9284,#9285,#9286,#9287,#9288,
#9289,#9290,#9291)) ;
#9553 = CLOSED_SHELL('',(#9292,#9293,#9294,#9295,#9296,#9297,#9298,#9299)) ;
#9554 = CLOSED_SHELL('',(#9300,#9301,#9302,#9303,#9304,#9305,#9306,#9307)) ;
#9555 = CLOSED_SHELL('',(#9308,#9309,#9310,#9311,#9312,#9313,#9314,#9315,
#9316,#9317,#9318,#9319,#9320,#9321,#9322,#9323,#9324,#9325,#9326,#9327,
#9328,#9329,#9330,#9331,#9332,#9333,#9334,#9335,#9336,#9337,#9338,#9339,
#9340,#9341,#9342,#9343,#9344,#9345,#9346,#9347,#9348,#9349,#9350,#9351,
#9352,#9353,#9354,#9355,#9356,#9357,#9358,#9359,#9360,#9361,#9362,#9363,
#9364,#9365,#9366,#9367,#9368,#9369,#9370,#9371,#9372,#9373,#9374,#9375,
#9376,#9377,#9378,#9379,#9380,#9381,#9382,#9383,#9384,#9385,#9386,#9387,
#9388,#9389,#9390,#9391,#9392,#9393,#9394,#9395,#9396,#9397,#9398,#9399,
#9400,#9401,#9402,#9403,#9404,#9405,#9406,#9407,#9408,#9409,#9410,#9411,
#9412,#9413,#9414,#9415,#9416,#9417,#9418,#9419,#9420,#9421,#9422,#9423,
#9424,#9425,#9426,#9427,#9428,#9429,#9430,#9431,#9432,#9433,#9434,#9435,
#9436,#9437,#9438,#9439,#9440,#9441,#9442,#9443,#9444,#9445,#9446,#9447,
#9448,#9449,#9450,#9451,#9452,#9453,#9454,#9455,#9456,#9457,#9458,#9459,
#9460,#9461,#9462,#9463,#9464,#9465,#9466,#9467,#9468,#9469,#9470,#9471,
#9472,#9473,#9474,#9475,#9476,#9477,#9478,#9479,#9480,#9481,#9482,#9483)) ;
#9556 = CLOSED_SHELL('',(#9484,#9485,#9486,#9487,#9488,#9489,#9490,#9491,
#9492,#9493,#9494,#9495,#9496,#9497,#9498,#9499,#9500,#9501,#9502,#9503,
#9504,#9505,#9506,#9507,#9508,#9509)) ;
#9557 = CLOSED_SHELL('',(#9510,#9511,#9512,#9513,#9514,#9515,#9516,#9517,
#9518,#9519,#9520,#9521,#9522,#9523,#9524,#9525,#9526,#9527,#9528,#9529)) ;
#9558 = CLOSED_SHELL('',(#9530,#9531,#9532,#9533,#9534,#9535,#9536,#9537,
#9538,#9539,#9540,#9541)) ;
#9559 = DERIVED_UNIT_ELEMENT(#9593,1.) ;
#9560 = DERIVED_UNIT_ELEMENT(#18759,-3.) ;
#9561 = DERIVED_UNIT_ELEMENT(#9593,1.) ;
#9562 = DERIVED_UNIT_ELEMENT(#18759,-3.) ;
#9563 = DERIVED_UNIT_ELEMENT(#9593,1.) ;
#9564 = DERIVED_UNIT_ELEMENT(#18759,-3.) ;
#9565 = DERIVED_UNIT_ELEMENT(#9593,1.) ;
#9566 = DERIVED_UNIT_ELEMENT(#18759,-3.) ;
#9567 = DERIVED_UNIT_ELEMENT(#9593,1.) ;
#9568 = DERIVED_UNIT_ELEMENT(#18759,-3.) ;
#9569 = DERIVED_UNIT_ELEMENT(#9593,1.) ;
#9570 = DERIVED_UNIT_ELEMENT(#18759,-3.) ;
#9571 = DERIVED_UNIT_ELEMENT(#9593,1.) ;
#9572 = DERIVED_UNIT_ELEMENT(#18759,-3.) ;
#9573 = DERIVED_UNIT_ELEMENT(#9593,1.) ;
#9574 = DERIVED_UNIT_ELEMENT(#18759,-3.) ;
#9575 = DERIVED_UNIT_ELEMENT(#9593,1.) ;
#9576 = DERIVED_UNIT_ELEMENT(#18759,-3.) ;
#9577 = DERIVED_UNIT_ELEMENT(#9593,1.) ;
#9578 = DERIVED_UNIT_ELEMENT(#18759,-3.) ;
#9579 = DERIVED_UNIT_ELEMENT(#9593,1.) ;
#9580 = DERIVED_UNIT_ELEMENT(#18759,-3.) ;
#9581 = DERIVED_UNIT_ELEMENT(#9593,1.) ;
#9582 = DERIVED_UNIT_ELEMENT(#18759,-3.) ;
#9583 = DERIVED_UNIT_ELEMENT(#9593,1.) ;
#9584 = DERIVED_UNIT_ELEMENT(#18759,-3.) ;
#9585 = DERIVED_UNIT_ELEMENT(#9593,1.) ;
#9586 = DERIVED_UNIT_ELEMENT(#18759,-3.) ;
#9587 = DERIVED_UNIT_ELEMENT(#9593,1.) ;
#9588 = DERIVED_UNIT_ELEMENT(#18759,-3.) ;
#9589 = DERIVED_UNIT_ELEMENT(#9593,1.) ;
#9590 = DERIVED_UNIT_ELEMENT(#18759,-3.) ;
#9591 = DERIVED_UNIT_ELEMENT(#9593,1.) ;
#9592 = DERIVED_UNIT_ELEMENT(#18759,-3.) ;
#9593 = (
MASS_UNIT()
NAMED_UNIT(*)
SI_UNIT(.KILO.,.GRAM.)
) ;
#9594 = DERIVED_UNIT((#9559,#9560)) ;
#9595 = DERIVED_UNIT((#9561,#9562)) ;
#9596 = DERIVED_UNIT((#9563,#9564)) ;
#9597 = DERIVED_UNIT((#9565,#9566)) ;
#9598 = DERIVED_UNIT((#9567,#9568)) ;
#9599 = DERIVED_UNIT((#9569,#9570)) ;
#9600 = DERIVED_UNIT((#9571,#9572)) ;
#9601 = DERIVED_UNIT((#9573,#9574)) ;
#9602 = DERIVED_UNIT((#9575,#9576)) ;
#9603 = DERIVED_UNIT((#9577,#9578)) ;
#9604 = DERIVED_UNIT((#9579,#9580)) ;
#9605 = DERIVED_UNIT((#9581,#9582)) ;
#9606 = DERIVED_UNIT((#9583,#9584)) ;
#9607 = DERIVED_UNIT((#9585,#9586)) ;
#9608 = DERIVED_UNIT((#9587,#9588)) ;
#9609 = DERIVED_UNIT((#9589,#9590)) ;
#9610 = DERIVED_UNIT((#9591,#9592)) ;
#9611 = MEASURE_REPRESENTATION_ITEM('density measure',
POSITIVE_RATIO_MEASURE(7850.),#9594) ;
#9612 = MEASURE_REPRESENTATION_ITEM('density measure',
POSITIVE_RATIO_MEASURE(7850.),#9595) ;
#9613 = MEASURE_REPRESENTATION_ITEM('density measure',
POSITIVE_RATIO_MEASURE(7850.),#9596) ;
#9614 = MEASURE_REPRESENTATION_ITEM('density measure',
POSITIVE_RATIO_MEASURE(7850.),#9597) ;
#9615 = MEASURE_REPRESENTATION_ITEM('density measure',
POSITIVE_RATIO_MEASURE(7850.),#9598) ;
#9616 = MEASURE_REPRESENTATION_ITEM('density measure',
POSITIVE_RATIO_MEASURE(7850.),#9599) ;
#9617 = MEASURE_REPRESENTATION_ITEM('density measure',
POSITIVE_RATIO_MEASURE(7850.),#9600) ;
#9618 = MEASURE_REPRESENTATION_ITEM('density measure',
POSITIVE_RATIO_MEASURE(7850.),#9601) ;
#9619 = MEASURE_REPRESENTATION_ITEM('density measure',
POSITIVE_RATIO_MEASURE(7850.),#9602) ;
#9620 = MEASURE_REPRESENTATION_ITEM('density measure',
POSITIVE_RATIO_MEASURE(7850.),#9603) ;
#9621 = MEASURE_REPRESENTATION_ITEM('density measure',
POSITIVE_RATIO_MEASURE(7850.),#9604) ;
#9622 = MEASURE_REPRESENTATION_ITEM('density measure',
POSITIVE_RATIO_MEASURE(7850.),#9605) ;
#9623 = MEASURE_REPRESENTATION_ITEM('density measure',
POSITIVE_RATIO_MEASURE(7850.),#9606) ;
#9624 = MEASURE_REPRESENTATION_ITEM('density measure',
POSITIVE_RATIO_MEASURE(7850.),#9607) ;
#9625 = MEASURE_REPRESENTATION_ITEM('density measure',
POSITIVE_RATIO_MEASURE(7850.),#9608) ;
#9626 = MEASURE_REPRESENTATION_ITEM('density measure',
POSITIVE_RATIO_MEASURE(7850.),#9609) ;
#9627 = MEASURE_REPRESENTATION_ITEM('density measure',
POSITIVE_RATIO_MEASURE(7850.),#9610) ;
#9628 = PROPERTY_DEFINITION_REPRESENTATION(#9713,#9662) ;
#9629 = PROPERTY_DEFINITION_REPRESENTATION(#9714,#9663) ;
#9630 = PROPERTY_DEFINITION_REPRESENTATION(#9715,#9664) ;
#9631 = PROPERTY_DEFINITION_REPRESENTATION(#9716,#9665) ;
#9632 = PROPERTY_DEFINITION_REPRESENTATION(#9717,#9666) ;
#9633 = PROPERTY_DEFINITION_REPRESENTATION(#9718,#9667) ;
#9634 = PROPERTY_DEFINITION_REPRESENTATION(#9719,#9668) ;
#9635 = PROPERTY_DEFINITION_REPRESENTATION(#9720,#9669) ;
#9636 = PROPERTY_DEFINITION_REPRESENTATION(#9721,#9670) ;
#9637 = PROPERTY_DEFINITION_REPRESENTATION(#9722,#9671) ;
#9638 = PROPERTY_DEFINITION_REPRESENTATION(#9723,#9672) ;
#9639 = PROPERTY_DEFINITION_REPRESENTATION(#9724,#9673) ;
#9640 = PROPERTY_DEFINITION_REPRESENTATION(#9725,#9674) ;
#9641 = PROPERTY_DEFINITION_REPRESENTATION(#9726,#9675) ;
#9642 = PROPERTY_DEFINITION_REPRESENTATION(#9727,#9676) ;
#9643 = PROPERTY_DEFINITION_REPRESENTATION(#9728,#9677) ;
#9644 = PROPERTY_DEFINITION_REPRESENTATION(#9729,#9678) ;
#9645 = PROPERTY_DEFINITION_REPRESENTATION(#9730,#9679) ;
#9646 = PROPERTY_DEFINITION_REPRESENTATION(#9731,#9680) ;
#9647 = PROPERTY_DEFINITION_REPRESENTATION(#9732,#9681) ;
#9648 = PROPERTY_DEFINITION_REPRESENTATION(#9733,#9682) ;
#9649 = PROPERTY_DEFINITION_REPRESENTATION(#9734,#9683) ;
#9650 = PROPERTY_DEFINITION_REPRESENTATION(#9735,#9684) ;
#9651 = PROPERTY_DEFINITION_REPRESENTATION(#9736,#9685) ;
#9652 = PROPERTY_DEFINITION_REPRESENTATION(#9737,#9686) ;
#9653 = PROPERTY_DEFINITION_REPRESENTATION(#9738,#9687) ;
#9654 = PROPERTY_DEFINITION_REPRESENTATION(#9739,#9688) ;
#9655 = PROPERTY_DEFINITION_REPRESENTATION(#9740,#9689) ;
#9656 = PROPERTY_DEFINITION_REPRESENTATION(#9741,#9690) ;
#9657 = PROPERTY_DEFINITION_REPRESENTATION(#9742,#9691) ;
#9658 = PROPERTY_DEFINITION_REPRESENTATION(#9743,#9692) ;
#9659 = PROPERTY_DEFINITION_REPRESENTATION(#9744,#9693) ;
#9660 = PROPERTY_DEFINITION_REPRESENTATION(#9745,#9694) ;
#9661 = PROPERTY_DEFINITION_REPRESENTATION(#9746,#9695) ;
#9662 = REPRESENTATION('material name',(#9696),#18740) ;
#9663 = REPRESENTATION('density',(#9611),#18740) ;
#9664 = REPRESENTATION('material name',(#9697),#18741) ;
#9665 = REPRESENTATION('density',(#9612),#18741) ;
#9666 = REPRESENTATION('material name',(#9698),#18742) ;
#9667 = REPRESENTATION('density',(#9613),#18742) ;
#9668 = REPRESENTATION('material name',(#9699),#18743) ;
#9669 = REPRESENTATION('density',(#9614),#18743) ;
#9670 = REPRESENTATION('material name',(#9700),#18744) ;
#9671 = REPRESENTATION('density',(#9615),#18744) ;
#9672 = REPRESENTATION('material name',(#9701),#18745) ;
#9673 = REPRESENTATION('density',(#9616),#18745) ;
#9674 = REPRESENTATION('material name',(#9702),#18746) ;
#9675 = REPRESENTATION('density',(#9617),#18746) ;
#9676 = REPRESENTATION('material name',(#9703),#18747) ;
#9677 = REPRESENTATION('density',(#9618),#18747) ;
#9678 = REPRESENTATION('material name',(#9704),#18748) ;
#9679 = REPRESENTATION('density',(#9619),#18748) ;
#9680 = REPRESENTATION('material name',(#9705),#18749) ;
#9681 = REPRESENTATION('density',(#9620),#18749) ;
#9682 = REPRESENTATION('material name',(#9706),#18750) ;
#9683 = REPRESENTATION('density',(#9621),#18750) ;
#9684 = REPRESENTATION('material name',(#9707),#18751) ;
#9685 = REPRESENTATION('density',(#9622),#18751) ;
#9686 = REPRESENTATION('material name',(#9708),#18752) ;
#9687 = REPRESENTATION('density',(#9623),#18752) ;
#9688 = REPRESENTATION('material name',(#9709),#18753) ;
#9689 = REPRESENTATION('density',(#9624),#18753) ;
#9690 = REPRESENTATION('material name',(#9710),#18754) ;
#9691 = REPRESENTATION('density',(#9625),#18754) ;
#9692 = REPRESENTATION('material name',(#9711),#18755) ;
#9693 = REPRESENTATION('density',(#9626),#18755) ;
#9694 = REPRESENTATION('material name',(#9712),#18756) ;
#9695 = REPRESENTATION('density',(#9627),#18756) ;
#9696 = DESCRIPTIVE_REPRESENTATION_ITEM('Steel','Steel') ;
#9697 = DESCRIPTIVE_REPRESENTATION_ITEM('Steel','Steel') ;
#9698 = DESCRIPTIVE_REPRESENTATION_ITEM('Steel','Steel') ;
#9699 = DESCRIPTIVE_REPRESENTATION_ITEM('Steel','Steel') ;
#9700 = DESCRIPTIVE_REPRESENTATION_ITEM('Steel','Steel') ;
#9701 = DESCRIPTIVE_REPRESENTATION_ITEM('Steel','Steel') ;
#9702 = DESCRIPTIVE_REPRESENTATION_ITEM('Steel','Steel') ;
#9703 = DESCRIPTIVE_REPRESENTATION_ITEM('Steel','Steel') ;
#9704 = DESCRIPTIVE_REPRESENTATION_ITEM('Steel','Steel') ;
#9705 = DESCRIPTIVE_REPRESENTATION_ITEM('Steel','Steel') ;
#9706 = DESCRIPTIVE_REPRESENTATION_ITEM('Steel','Steel') ;
#9707 = DESCRIPTIVE_REPRESENTATION_ITEM('Steel','Steel') ;
#9708 = DESCRIPTIVE_REPRESENTATION_ITEM('Steel','Steel') ;
#9709 = DESCRIPTIVE_REPRESENTATION_ITEM('Steel','Steel') ;
#9710 = DESCRIPTIVE_REPRESENTATION_ITEM('Steel','Steel') ;
#9711 = DESCRIPTIVE_REPRESENTATION_ITEM('Steel','Steel') ;
#9712 = DESCRIPTIVE_REPRESENTATION_ITEM('Steel','Steel') ;
#9713 = PROPERTY_DEFINITION('material property','material name',#18876) ;
#9714 = PROPERTY_DEFINITION('material property','density of part',#18876) ;
#9715 = PROPERTY_DEFINITION('material property','material name',#18877) ;
#9716 = PROPERTY_DEFINITION('material property','density of part',#18877) ;
#9717 = PROPERTY_DEFINITION('material property','material name',#18878) ;
#9718 = PROPERTY_DEFINITION('material property','density of part',#18878) ;
#9719 = PROPERTY_DEFINITION('material property','material name',#18879) ;
#9720 = PROPERTY_DEFINITION('material property','density of part',#18879) ;
#9721 = PROPERTY_DEFINITION('material property','material name',#18880) ;
#9722 = PROPERTY_DEFINITION('material property','density of part',#18880) ;
#9723 = PROPERTY_DEFINITION('material property','material name',#18881) ;
#9724 = PROPERTY_DEFINITION('material property','density of part',#18881) ;
#9725 = PROPERTY_DEFINITION('material property','material name',#18882) ;
#9726 = PROPERTY_DEFINITION('material property','density of part',#18882) ;
#9727 = PROPERTY_DEFINITION('material property','material name',#18883) ;
#9728 = PROPERTY_DEFINITION('material property','density of part',#18883) ;
#9729 = PROPERTY_DEFINITION('material property','material name',#18884) ;
#9730 = PROPERTY_DEFINITION('material property','density of part',#18884) ;
#9731 = PROPERTY_DEFINITION('material property','material name',#18885) ;
#9732 = PROPERTY_DEFINITION('material property','density of part',#18885) ;
#9733 = PROPERTY_DEFINITION('material property','material name',#18886) ;
#9734 = PROPERTY_DEFINITION('material property','density of part',#18886) ;
#9735 = PROPERTY_DEFINITION('material property','material name',#18887) ;
#9736 = PROPERTY_DEFINITION('material property','density of part',#18887) ;
#9737 = PROPERTY_DEFINITION('material property','material name',#18888) ;
#9738 = PROPERTY_DEFINITION('material property','density of part',#18888) ;
#9739 = PROPERTY_DEFINITION('material property','material name',#18889) ;
#9740 = PROPERTY_DEFINITION('material property','density of part',#18889) ;
#9741 = PROPERTY_DEFINITION('material property','material name',#18890) ;
#9742 = PROPERTY_DEFINITION('material property','density of part',#18890) ;
#9743 = PROPERTY_DEFINITION('material property','material name',#18891) ;
#9744 = PROPERTY_DEFINITION('material property','density of part',#18891) ;
#9745 = PROPERTY_DEFINITION('material property','material name',#18892) ;
#9746 = PROPERTY_DEFINITION('material property','density of part',#18892) ;
#9747 = AXIS2_PLACEMENT_3D('',#13422,#10715,#10716) ;
#9748 = AXIS2_PLACEMENT_3D('',#13423,#10717,#10718) ;
#9749 = AXIS2_PLACEMENT_3D('',#13424,#10719,#10720) ;
#9750 = AXIS2_PLACEMENT_3D('',#13426,#10721,#10722) ;
#9751 = AXIS2_PLACEMENT_3D('',#13429,#10724,#10725) ;
#9752 = AXIS2_PLACEMENT_3D('',#13430,#10726,#10727) ;
#9753 = AXIS2_PLACEMENT_3D('',#13440,#10732,#10733) ;
#9754 = AXIS2_PLACEMENT_3D('',#13441,#10734,#10735) ;
#9755 = AXIS2_PLACEMENT_3D('',#13444,#10737,#10738) ;
#9756 = AXIS2_PLACEMENT_3D('',#13445,#10739,#10740) ;
#9757 = AXIS2_PLACEMENT_3D('',#13447,#10741,#10742) ;
#9758 = AXIS2_PLACEMENT_3D('',#13450,#10744,#10745) ;
#9759 = AXIS2_PLACEMENT_3D('',#13451,#10746,#10747) ;
#9760 = AXIS2_PLACEMENT_3D('',#13461,#10752,#10753) ;
#9761 = AXIS2_PLACEMENT_3D('',#13462,#10754,#10755) ;
#9762 = AXIS2_PLACEMENT_3D('',#13465,#10757,#10758) ;
#9763 = AXIS2_PLACEMENT_3D('',#13466,#10759,#10760) ;
#9764 = AXIS2_PLACEMENT_3D('',#13468,#10761,#10762) ;
#9765 = AXIS2_PLACEMENT_3D('',#13471,#10764,#10765) ;
#9766 = AXIS2_PLACEMENT_3D('',#13472,#10766,#10767) ;
#9767 = AXIS2_PLACEMENT_3D('',#13482,#10772,#10773) ;
#9768 = AXIS2_PLACEMENT_3D('',#13483,#10774,#10775) ;
#9769 = AXIS2_PLACEMENT_3D('',#13486,#10777,#10778) ;
#9770 = AXIS2_PLACEMENT_3D('',#13487,#10779,#10780) ;
#9771 = AXIS2_PLACEMENT_3D('',#13489,#10781,#10782) ;
#9772 = AXIS2_PLACEMENT_3D('',#13492,#10784,#10785) ;
#9773 = AXIS2_PLACEMENT_3D('',#13493,#10786,#10787) ;
#9774 = AXIS2_PLACEMENT_3D('',#13503,#10792,#10793) ;
#9775 = AXIS2_PLACEMENT_3D('',#13504,#10794,#10795) ;
#9776 = AXIS2_PLACEMENT_3D('',#13507,#10797,#10798) ;
#9777 = AXIS2_PLACEMENT_3D('',#13508,#10799,#10800) ;
#9778 = AXIS2_PLACEMENT_3D('',#13511,#10802,#10803) ;
#9779 = AXIS2_PLACEMENT_3D('',#13512,#10804,#10805) ;
#9780 = AXIS2_PLACEMENT_3D('',#13516,#10807,#10808) ;
#9781 = AXIS2_PLACEMENT_3D('',#13553,#10809,#10810) ;
#9782 = AXIS2_PLACEMENT_3D('',#13554,#10811,#10812) ;
#9783 = AXIS2_PLACEMENT_3D('',#13557,#10814,#10815) ;
#9784 = AXIS2_PLACEMENT_3D('',#13558,#10816,#10817) ;
#9785 = AXIS2_PLACEMENT_3D('',#13562,#10819,#10820) ;
#9786 = AXIS2_PLACEMENT_3D('',#13599,#10821,#10822) ;
#9787 = AXIS2_PLACEMENT_3D('',#13600,#10823,#10824) ;
#9788 = AXIS2_PLACEMENT_3D('',#13603,#10826,#10827) ;
#9789 = AXIS2_PLACEMENT_3D('',#13604,#10828,#10829) ;
#9790 = AXIS2_PLACEMENT_3D('',#13607,#10831,#10832) ;
#9791 = AXIS2_PLACEMENT_3D('',#13608,#10833,#10834) ;
#9792 = AXIS2_PLACEMENT_3D('',#13611,#10836,#10837) ;
#9793 = AXIS2_PLACEMENT_3D('',#13612,#10838,#10839) ;
#9794 = AXIS2_PLACEMENT_3D('',#13615,#10841,#10842) ;
#9795 = AXIS2_PLACEMENT_3D('',#13616,#10843,#10844) ;
#9796 = AXIS2_PLACEMENT_3D('',#13619,#10846,#10847) ;
#9797 = AXIS2_PLACEMENT_3D('',#13622,#10849,#10850) ;
#9798 = AXIS2_PLACEMENT_3D('',#13625,#10852,#10853) ;
#9799 = AXIS2_PLACEMENT_3D('',#13628,#10855,#10856) ;
#9800 = AXIS2_PLACEMENT_3D('',#13636,#10857,#10858) ;
#9801 = AXIS2_PLACEMENT_3D('',#13638,#10859,#10860) ;
#9802 = AXIS2_PLACEMENT_3D('',#13641,#10862,#10863) ;
#9803 = AXIS2_PLACEMENT_3D('',#13642,#10864,#10865) ;
#9804 = AXIS2_PLACEMENT_3D('',#13645,#10867,#10868) ;
#9805 = AXIS2_PLACEMENT_3D('',#13653,#10869,#10870) ;
#9806 = AXIS2_PLACEMENT_3D('',#13655,#10871,#10872) ;
#9807 = AXIS2_PLACEMENT_3D('',#13658,#10874,#10875) ;
#9808 = AXIS2_PLACEMENT_3D('',#13659,#10876,#10877) ;
#9809 = AXIS2_PLACEMENT_3D('',#13662,#10879,#10880) ;
#9810 = AXIS2_PLACEMENT_3D('',#13740,#10882,#10883) ;
#9811 = AXIS2_PLACEMENT_3D('',#13742,#10884,#10885) ;
#9812 = AXIS2_PLACEMENT_3D('',#13745,#10887,#10888) ;
#9813 = AXIS2_PLACEMENT_3D('',#13746,#10889,#10890) ;
#9814 = AXIS2_PLACEMENT_3D('',#13747,#10891,#10892) ;
#9815 = AXIS2_PLACEMENT_3D('',#13825,#10894,#10895) ;
#9816 = AXIS2_PLACEMENT_3D('',#13827,#10896,#10897) ;
#9817 = AXIS2_PLACEMENT_3D('',#13830,#10899,#10900) ;
#9818 = AXIS2_PLACEMENT_3D('',#13831,#10901,#10902) ;
#9819 = AXIS2_PLACEMENT_3D('',#13832,#10903,#10904) ;
#9820 = AXIS2_PLACEMENT_3D('',#13834,#10905,#10906) ;
#9821 = AXIS2_PLACEMENT_3D('',#13837,#10908,#10909) ;
#9822 = AXIS2_PLACEMENT_3D('',#13838,#10910,#10911) ;
#9823 = AXIS2_PLACEMENT_3D('',#13840,#10912,#10913) ;
#9824 = AXIS2_PLACEMENT_3D('',#13843,#10915,#10916) ;
#9825 = AXIS2_PLACEMENT_3D('',#13844,#10917,#10918) ;
#9826 = AXIS2_PLACEMENT_3D('',#13849,#10920,#10921) ;
#9827 = AXIS2_PLACEMENT_3D('',#13852,#10923,#10924) ;
#9828 = AXIS2_PLACEMENT_3D('',#13853,#10925,#10926) ;
#9829 = AXIS2_PLACEMENT_3D('',#13858,#10928,#10929) ;
#9830 = AXIS2_PLACEMENT_3D('',#13861,#10931,#10932) ;
#9831 = AXIS2_PLACEMENT_3D('',#13862,#10933,#10934) ;
#9832 = AXIS2_PLACEMENT_3D('',#13868,#10938,#10939) ;
#9833 = AXIS2_PLACEMENT_3D('',#13870,#10940,#10941) ;
#9834 = AXIS2_PLACEMENT_3D('',#13876,#10945,#10946) ;
#9835 = AXIS2_PLACEMENT_3D('',#13882,#10950,#10951) ;
#9836 = AXIS2_PLACEMENT_3D('',#13884,#10952,#10953) ;
#9837 = AXIS2_PLACEMENT_3D('',#13890,#10957,#10958) ;
#9838 = AXIS2_PLACEMENT_3D('',#13899,#10963,#10964) ;
#9839 = AXIS2_PLACEMENT_3D('',#13909,#10970,#10971) ;
#9840 = AXIS2_PLACEMENT_3D('',#13943,#10990,#10991) ;
#9841 = AXIS2_PLACEMENT_3D('',#13949,#10995,#10996) ;
#9842 = AXIS2_PLACEMENT_3D('',#13957,#11001,#11002) ;
#9843 = AXIS2_PLACEMENT_3D('',#13959,#11003,#11004) ;
#9844 = AXIS2_PLACEMENT_3D('',#13963,#11006,#11007) ;
#9845 = AXIS2_PLACEMENT_3D('',#13966,#11009,#11010) ;
#9846 = AXIS2_PLACEMENT_3D('',#13967,#11011,#11012) ;
#9847 = AXIS2_PLACEMENT_3D('',#13969,#11013,#11014) ;
#9848 = AXIS2_PLACEMENT_3D('',#13972,#11016,#11017) ;
#9849 = AXIS2_PLACEMENT_3D('',#13973,#11018,#11019) ;
#9850 = AXIS2_PLACEMENT_3D('',#13974,#11020,#11021) ;
#9851 = AXIS2_PLACEMENT_3D('',#13976,#11023,#11024) ;
#9852 = AXIS2_PLACEMENT_3D('',#13977,#11025,#11026) ;
#9853 = AXIS2_PLACEMENT_3D('',#14009,#11044,#11045) ;
#9854 = AXIS2_PLACEMENT_3D('',#14010,#11046,#11047) ;
#9855 = AXIS2_PLACEMENT_3D('',#14011,#11048,#11049) ;
#9856 = AXIS2_PLACEMENT_3D('',#14013,#11051,#11052) ;
#9857 = AXIS2_PLACEMENT_3D('',#14017,#11055,#11056) ;
#9858 = AXIS2_PLACEMENT_3D('',#14018,#11057,#11058) ;
#9859 = AXIS2_PLACEMENT_3D('',#14019,#11059,#11060) ;
#9860 = AXIS2_PLACEMENT_3D('',#14020,#11061,#11062) ;
#9861 = AXIS2_PLACEMENT_3D('',#14029,#11067,#11068) ;
#9862 = AXIS2_PLACEMENT_3D('',#14035,#11072,#11073) ;
#9863 = AXIS2_PLACEMENT_3D('',#14039,#11076,#11077) ;
#9864 = AXIS2_PLACEMENT_3D('',#14041,#11078,#11079) ;
#9865 = AXIS2_PLACEMENT_3D('',#14044,#11081,#11082) ;
#9866 = AXIS2_PLACEMENT_3D('',#14045,#11083,#11084) ;
#9867 = AXIS2_PLACEMENT_3D('',#14046,#11085,#11086) ;
#9868 = AXIS2_PLACEMENT_3D('',#14047,#11087,#11088) ;
#9869 = AXIS2_PLACEMENT_3D('',#14048,#11089,#11090) ;
#9870 = AXIS2_PLACEMENT_3D('',#14049,#11091,#11092) ;
#9871 = AXIS2_PLACEMENT_3D('',#14050,#11093,#11094) ;
#9872 = AXIS2_PLACEMENT_3D('',#14051,#11095,#11096) ;
#9873 = AXIS2_PLACEMENT_3D('',#14053,#11098,#11099) ;
#9874 = AXIS2_PLACEMENT_3D('',#14057,#11102,#11103) ;
#9875 = AXIS2_PLACEMENT_3D('',#14058,#11104,#11105) ;
#9876 = AXIS2_PLACEMENT_3D('',#14059,#11106,#11107) ;
#9877 = AXIS2_PLACEMENT_3D('',#14060,#11108,#11109) ;
#9878 = AXIS2_PLACEMENT_3D('',#14069,#11114,#11115) ;
#9879 = AXIS2_PLACEMENT_3D('',#14075,#11119,#11120) ;
#9880 = AXIS2_PLACEMENT_3D('',#14079,#11123,#11124) ;
#9881 = AXIS2_PLACEMENT_3D('',#14085,#11128,#11129) ;
#9882 = AXIS2_PLACEMENT_3D('',#14091,#11133,#11134) ;
#9883 = AXIS2_PLACEMENT_3D('',#14094,#11137,#11138) ;
#9884 = AXIS2_PLACEMENT_3D('',#14096,#11140,#11141) ;
#9885 = AXIS2_PLACEMENT_3D('',#14102,#11145,#11146) ;
#9886 = AXIS2_PLACEMENT_3D('',#14105,#11149,#11150) ;
#9887 = AXIS2_PLACEMENT_3D('',#14109,#11153,#11154) ;
#9888 = AXIS2_PLACEMENT_3D('',#14113,#11157,#11158) ;
#9889 = AXIS2_PLACEMENT_3D('',#14122,#11165,#11166) ;
#9890 = AXIS2_PLACEMENT_3D('',#14128,#11170,#11171) ;
#9891 = AXIS2_PLACEMENT_3D('',#14131,#11174,#11175) ;
#9892 = AXIS2_PLACEMENT_3D('',#14135,#11178,#11179) ;
#9893 = AXIS2_PLACEMENT_3D('',#14140,#11183,#11184) ;
#9894 = AXIS2_PLACEMENT_3D('',#14142,#11186,#11187) ;
#9895 = AXIS2_PLACEMENT_3D('',#14144,#11189,#11190) ;
#9896 = AXIS2_PLACEMENT_3D('',#14146,#11192,#11193) ;
#9897 = AXIS2_PLACEMENT_3D('',#14148,#11195,#11196) ;
#9898 = AXIS2_PLACEMENT_3D('',#14152,#11199,#11200) ;
#9899 = AXIS2_PLACEMENT_3D('',#14156,#11203,#11204) ;
#9900 = AXIS2_PLACEMENT_3D('',#14158,#11206,#11207) ;
#9901 = AXIS2_PLACEMENT_3D('',#14160,#11209,#11210) ;
#9902 = AXIS2_PLACEMENT_3D('',#14161,#11211,#11212) ;
#9903 = AXIS2_PLACEMENT_3D('',#14163,#11214,#11215) ;
#9904 = AXIS2_PLACEMENT_3D('',#14165,#11217,#11218) ;
#9905 = AXIS2_PLACEMENT_3D('',#14166,#11219,#11220) ;
#9906 = AXIS2_PLACEMENT_3D('',#14167,#11221,#11222) ;
#9907 = AXIS2_PLACEMENT_3D('',#14169,#11223,#11224) ;
#9908 = AXIS2_PLACEMENT_3D('',#14172,#11226,#11227) ;
#9909 = AXIS2_PLACEMENT_3D('',#14173,#11228,#11229) ;
#9910 = AXIS2_PLACEMENT_3D('',#14175,#11230,#11231) ;
#9911 = AXIS2_PLACEMENT_3D('',#14178,#11233,#11234) ;
#9912 = AXIS2_PLACEMENT_3D('',#14179,#11235,#11236) ;
#9913 = AXIS2_PLACEMENT_3D('',#14188,#11241,#11242) ;
#9914 = AXIS2_PLACEMENT_3D('',#14198,#11248,#11249) ;
#9915 = AXIS2_PLACEMENT_3D('',#14204,#11253,#11254) ;
#9916 = AXIS2_PLACEMENT_3D('',#14206,#11256,#11257) ;
#9917 = AXIS2_PLACEMENT_3D('',#14212,#11261,#11262) ;
#9918 = AXIS2_PLACEMENT_3D('',#14214,#11263,#11264) ;
#9919 = AXIS2_PLACEMENT_3D('',#14217,#11266,#11267) ;
#9920 = AXIS2_PLACEMENT_3D('',#14218,#11268,#11269) ;
#9921 = AXIS2_PLACEMENT_3D('',#14220,#11270,#11271) ;
#9922 = AXIS2_PLACEMENT_3D('',#14223,#11273,#11274) ;
#9923 = AXIS2_PLACEMENT_3D('',#14224,#11275,#11276) ;
#9924 = AXIS2_PLACEMENT_3D('',#14227,#11277,#11278) ;
#9925 = AXIS2_PLACEMENT_3D('',#14231,#11280,#11281) ;
#9926 = AXIS2_PLACEMENT_3D('',#14235,#11283,#11284) ;
#9927 = AXIS2_PLACEMENT_3D('',#14239,#11286,#11287) ;
#9928 = AXIS2_PLACEMENT_3D('',#14244,#11290,#11291) ;
#9929 = AXIS2_PLACEMENT_3D('',#14250,#11294,#11295) ;
#9930 = AXIS2_PLACEMENT_3D('',#14254,#11297,#11298) ;
#9931 = AXIS2_PLACEMENT_3D('',#14258,#11300,#11301) ;
#9932 = AXIS2_PLACEMENT_3D('',#14260,#11303,#11304) ;
#9933 = AXIS2_PLACEMENT_3D('',#14269,#11309,#11310) ;
#9934 = AXIS2_PLACEMENT_3D('',#14275,#11314,#11315) ;
#9935 = AXIS2_PLACEMENT_3D('',#14282,#11320,#11321) ;
#9936 = AXIS2_PLACEMENT_3D('',#14284,#11323,#11324) ;
#9937 = AXIS2_PLACEMENT_3D('',#14288,#11327,#11328) ;
#9938 = AXIS2_PLACEMENT_3D('',#14290,#11329,#11330) ;
#9939 = AXIS2_PLACEMENT_3D('',#14292,#11332,#11333) ;
#9940 = AXIS2_PLACEMENT_3D('',#14295,#11335,#11336) ;
#9941 = AXIS2_PLACEMENT_3D('',#14296,#11337,#11338) ;
#9942 = AXIS2_PLACEMENT_3D('',#14299,#11339,#11340) ;
#9943 = AXIS2_PLACEMENT_3D('',#14303,#11342,#11343) ;
#9944 = AXIS2_PLACEMENT_3D('',#14305,#11345,#11346) ;
#9945 = AXIS2_PLACEMENT_3D('',#14308,#11347,#11348) ;
#9946 = AXIS2_PLACEMENT_3D('',#14309,#11349,#11350) ;
#9947 = AXIS2_PLACEMENT_3D('',#14310,#11351,#11352) ;
#9948 = AXIS2_PLACEMENT_3D('',#14311,#11353,#11354) ;
#9949 = AXIS2_PLACEMENT_3D('',#14314,#11355,#11356) ;
#9950 = AXIS2_PLACEMENT_3D('',#14317,#11359,#11360) ;
#9951 = AXIS2_PLACEMENT_3D('',#14320,#11361,#11362) ;
#9952 = AXIS2_PLACEMENT_3D('',#14321,#11363,#11364) ;
#9953 = AXIS2_PLACEMENT_3D('',#14322,#11365,#11366) ;
#9954 = AXIS2_PLACEMENT_3D('',#14323,#11367,#11368) ;
#9955 = AXIS2_PLACEMENT_3D('',#14326,#11369,#11370) ;
#9956 = AXIS2_PLACEMENT_3D('',#14329,#11373,#11374) ;
#9957 = AXIS2_PLACEMENT_3D('',#14332,#11375,#11376) ;
#9958 = AXIS2_PLACEMENT_3D('',#14333,#11377,#11378) ;
#9959 = AXIS2_PLACEMENT_3D('',#14334,#11379,#11380) ;
#9960 = AXIS2_PLACEMENT_3D('',#14335,#11381,#11382) ;
#9961 = AXIS2_PLACEMENT_3D('',#14338,#11383,#11384) ;
#9962 = AXIS2_PLACEMENT_3D('',#14341,#11387,#11388) ;
#9963 = AXIS2_PLACEMENT_3D('',#14342,#11389,#11390) ;
#9964 = AXIS2_PLACEMENT_3D('',#14343,#11391,#11392) ;
#9965 = AXIS2_PLACEMENT_3D('',#14344,#11393,#11394) ;
#9966 = AXIS2_PLACEMENT_3D('',#14347,#11397,#11398) ;
#9967 = AXIS2_PLACEMENT_3D('',#14349,#11400,#11401) ;
#9968 = AXIS2_PLACEMENT_3D('',#14351,#11403,#11404) ;
#9969 = AXIS2_PLACEMENT_3D('',#14353,#11406,#11407) ;
#9970 = AXIS2_PLACEMENT_3D('',#14354,#11408,#11409) ;
#9971 = AXIS2_PLACEMENT_3D('',#14360,#11413,#11414) ;
#9972 = AXIS2_PLACEMENT_3D('',#14363,#11416,#11417) ;
#9973 = AXIS2_PLACEMENT_3D('',#14364,#11418,#11419) ;
#9974 = AXIS2_PLACEMENT_3D('',#14366,#11421,#11422) ;
#9975 = AXIS2_PLACEMENT_3D('',#14368,#11424,#11425) ;
#9976 = AXIS2_PLACEMENT_3D('',#14372,#11428,#11429) ;
#9977 = AXIS2_PLACEMENT_3D('',#14373,#11430,#11431) ;
#9978 = AXIS2_PLACEMENT_3D('',#14374,#11432,#11433) ;
#9979 = AXIS2_PLACEMENT_3D('',#14375,#11434,#11435) ;
#9980 = AXIS2_PLACEMENT_3D('',#14377,#11437,#11438) ;
#9981 = AXIS2_PLACEMENT_3D('',#14379,#11440,#11441) ;
#9982 = AXIS2_PLACEMENT_3D('',#14381,#11443,#11444) ;
#9983 = AXIS2_PLACEMENT_3D('',#14382,#11445,#11446) ;
#9984 = AXIS2_PLACEMENT_3D('',#14383,#11447,#11448) ;
#9985 = AXIS2_PLACEMENT_3D('',#14385,#11449,#11450) ;
#9986 = AXIS2_PLACEMENT_3D('',#14388,#11452,#11453) ;
#9987 = AXIS2_PLACEMENT_3D('',#14389,#11454,#11455) ;
#9988 = AXIS2_PLACEMENT_3D('',#14391,#11456,#11457) ;
#9989 = AXIS2_PLACEMENT_3D('',#14394,#11459,#11460) ;
#9990 = AXIS2_PLACEMENT_3D('',#14395,#11461,#11462) ;
#9991 = AXIS2_PLACEMENT_3D('',#14397,#11463,#11464) ;
#9992 = AXIS2_PLACEMENT_3D('',#14400,#11466,#11467) ;
#9993 = AXIS2_PLACEMENT_3D('',#14401,#11468,#11469) ;
#9994 = AXIS2_PLACEMENT_3D('',#14403,#11470,#11471) ;
#9995 = AXIS2_PLACEMENT_3D('',#14406,#11473,#11474) ;
#9996 = AXIS2_PLACEMENT_3D('',#14407,#11475,#11476) ;
#9997 = AXIS2_PLACEMENT_3D('',#14416,#11481,#11482) ;
#9998 = AXIS2_PLACEMENT_3D('',#14418,#11483,#11484) ;
#9999 = AXIS2_PLACEMENT_3D('',#14420,#11485,#11486) ;
#10000 = AXIS2_PLACEMENT_3D('',#14422,#11488,#11489) ;
#10001 = AXIS2_PLACEMENT_3D('',#14428,#11493,#11494) ;
#10002 = AXIS2_PLACEMENT_3D('',#14429,#11495,#11496) ;
#10003 = AXIS2_PLACEMENT_3D('',#14430,#11497,#11498) ;
#10004 = AXIS2_PLACEMENT_3D('',#14431,#11499,#11500) ;
#10005 = AXIS2_PLACEMENT_3D('',#14432,#11501,#11502) ;
#10006 = AXIS2_PLACEMENT_3D('',#14433,#11503,#11504) ;
#10007 = AXIS2_PLACEMENT_3D('',#14435,#11505,#11506) ;
#10008 = AXIS2_PLACEMENT_3D('',#14438,#11508,#11509) ;
#10009 = AXIS2_PLACEMENT_3D('',#14439,#11510,#11511) ;
#10010 = AXIS2_PLACEMENT_3D('',#14441,#11512,#11513) ;
#10011 = AXIS2_PLACEMENT_3D('',#14444,#11515,#11516) ;
#10012 = AXIS2_PLACEMENT_3D('',#14445,#11517,#11518) ;
#10013 = AXIS2_PLACEMENT_3D('',#14447,#11519,#11520) ;
#10014 = AXIS2_PLACEMENT_3D('',#14450,#11522,#11523) ;
#10015 = AXIS2_PLACEMENT_3D('',#14451,#11524,#11525) ;
#10016 = AXIS2_PLACEMENT_3D('',#14460,#11530,#11531) ;
#10017 = AXIS2_PLACEMENT_3D('',#14462,#11532,#11533) ;
#10018 = AXIS2_PLACEMENT_3D('',#14464,#11534,#11535) ;
#10019 = AXIS2_PLACEMENT_3D('',#14466,#11537,#11538) ;
#10020 = AXIS2_PLACEMENT_3D('',#14472,#11542,#11543) ;
#10021 = AXIS2_PLACEMENT_3D('',#14473,#11544,#11545) ;
#10022 = AXIS2_PLACEMENT_3D('',#14474,#11546,#11547) ;
#10023 = AXIS2_PLACEMENT_3D('',#14475,#11548,#11549) ;
#10024 = AXIS2_PLACEMENT_3D('',#14476,#11550,#11551) ;
#10025 = AXIS2_PLACEMENT_3D('',#14477,#11552,#11553) ;
#10026 = AXIS2_PLACEMENT_3D('',#14478,#11554,#11555) ;
#10027 = AXIS2_PLACEMENT_3D('',#14480,#11556,#11557) ;
#10028 = AXIS2_PLACEMENT_3D('',#14483,#11559,#11560) ;
#10029 = AXIS2_PLACEMENT_3D('',#14484,#11561,#11562) ;
#10030 = AXIS2_PLACEMENT_3D('',#14486,#11563,#11564) ;
#10031 = AXIS2_PLACEMENT_3D('',#14489,#11566,#11567) ;
#10032 = AXIS2_PLACEMENT_3D('',#14490,#11568,#11569) ;
#10033 = AXIS2_PLACEMENT_3D('',#14492,#11570,#11571) ;
#10034 = AXIS2_PLACEMENT_3D('',#14495,#11573,#11574) ;
#10035 = AXIS2_PLACEMENT_3D('',#14496,#11575,#11576) ;
#10036 = AXIS2_PLACEMENT_3D('',#14498,#11577,#11578) ;
#10037 = AXIS2_PLACEMENT_3D('',#14501,#11580,#11581) ;
#10038 = AXIS2_PLACEMENT_3D('',#14502,#11582,#11583) ;
#10039 = AXIS2_PLACEMENT_3D('',#14504,#11584,#11585) ;
#10040 = AXIS2_PLACEMENT_3D('',#14507,#11587,#11588) ;
#10041 = AXIS2_PLACEMENT_3D('',#14508,#11589,#11590) ;
#10042 = AXIS2_PLACEMENT_3D('',#14517,#11595,#11596) ;
#10043 = AXIS2_PLACEMENT_3D('',#14519,#11597,#11598) ;
#10044 = AXIS2_PLACEMENT_3D('',#14521,#11599,#11600) ;
#10045 = AXIS2_PLACEMENT_3D('',#14523,#11602,#11603) ;
#10046 = AXIS2_PLACEMENT_3D('',#14529,#11607,#11608) ;
#10047 = AXIS2_PLACEMENT_3D('',#14530,#11609,#11610) ;
#10048 = AXIS2_PLACEMENT_3D('',#14531,#11611,#11612) ;
#10049 = AXIS2_PLACEMENT_3D('',#14532,#11613,#11614) ;
#10050 = AXIS2_PLACEMENT_3D('',#14533,#11615,#11616) ;
#10051 = AXIS2_PLACEMENT_3D('',#14534,#11617,#11618) ;
#10052 = AXIS2_PLACEMENT_3D('',#14536,#11619,#11620) ;
#10053 = AXIS2_PLACEMENT_3D('',#14539,#11622,#11623) ;
#10054 = AXIS2_PLACEMENT_3D('',#14540,#11624,#11625) ;
#10055 = AXIS2_PLACEMENT_3D('',#14542,#11626,#11627) ;
#10056 = AXIS2_PLACEMENT_3D('',#14545,#11629,#11630) ;
#10057 = AXIS2_PLACEMENT_3D('',#14546,#11631,#11632) ;
#10058 = AXIS2_PLACEMENT_3D('',#14548,#11633,#11634) ;
#10059 = AXIS2_PLACEMENT_3D('',#14551,#11636,#11637) ;
#10060 = AXIS2_PLACEMENT_3D('',#14552,#11638,#11639) ;
#10061 = AXIS2_PLACEMENT_3D('',#14561,#11644,#11645) ;
#10062 = AXIS2_PLACEMENT_3D('',#14563,#11646,#11647) ;
#10063 = AXIS2_PLACEMENT_3D('',#14565,#11648,#11649) ;
#10064 = AXIS2_PLACEMENT_3D('',#14567,#11651,#11652) ;
#10065 = AXIS2_PLACEMENT_3D('',#14573,#11656,#11657) ;
#10066 = AXIS2_PLACEMENT_3D('',#14574,#11658,#11659) ;
#10067 = AXIS2_PLACEMENT_3D('',#14575,#11660,#11661) ;
#10068 = AXIS2_PLACEMENT_3D('',#14576,#11662,#11663) ;
#10069 = AXIS2_PLACEMENT_3D('',#14577,#11664,#11665) ;
#10070 = AXIS2_PLACEMENT_3D('',#14578,#11666,#11667) ;
#10071 = AXIS2_PLACEMENT_3D('',#14579,#11668,#11669) ;
#10072 = AXIS2_PLACEMENT_3D('',#14584,#11671,#11672) ;
#10073 = AXIS2_PLACEMENT_3D('',#14589,#11673,#11674) ;
#10074 = AXIS2_PLACEMENT_3D('',#14594,#11676,#11677) ;
#10075 = AXIS2_PLACEMENT_3D('',#14616,#11678,#11679) ;
#10076 = AXIS2_PLACEMENT_3D('',#14636,#11680,#11681) ;
#10077 = AXIS2_PLACEMENT_3D('',#14638,#11682,#11683) ;
#10078 = AXIS2_PLACEMENT_3D('',#14641,#11685,#11686) ;
#10079 = AXIS2_PLACEMENT_3D('',#14642,#11687,#11688) ;
#10080 = AXIS2_PLACEMENT_3D('',#14644,#11689,#11690) ;
#10081 = AXIS2_PLACEMENT_3D('',#14645,#11691,#11692) ;
#10082 = AXIS2_PLACEMENT_3D('',#14648,#11694,#11695) ;
#10083 = AXIS2_PLACEMENT_3D('',#14649,#11696,#11697) ;
#10084 = AXIS2_PLACEMENT_3D('',#14651,#11698,#11699) ;
#10085 = AXIS2_PLACEMENT_3D('',#14652,#11700,#11701) ;
#10086 = AXIS2_PLACEMENT_3D('',#14655,#11703,#11704) ;
#10087 = AXIS2_PLACEMENT_3D('',#14656,#11705,#11706) ;
#10088 = AXIS2_PLACEMENT_3D('',#14658,#11707,#11708) ;
#10089 = AXIS2_PLACEMENT_3D('',#14659,#11709,#11710) ;
#10090 = AXIS2_PLACEMENT_3D('',#14661,#11711,#11712) ;
#10091 = AXIS2_PLACEMENT_3D('',#14663,#11714,#11715) ;
#10092 = AXIS2_PLACEMENT_3D('',#14665,#11716,#11717) ;
#10093 = AXIS2_PLACEMENT_3D('',#14666,#11718,#11719) ;
#10094 = AXIS2_PLACEMENT_3D('',#14672,#11721,#11722) ;
#10095 = AXIS2_PLACEMENT_3D('',#14673,#11723,#11724) ;
#10096 = AXIS2_PLACEMENT_3D('',#14674,#11725,#11726) ;
#10097 = AXIS2_PLACEMENT_3D('',#14675,#11727,#11728) ;
#10098 = AXIS2_PLACEMENT_3D('',#14676,#11729,#11730) ;
#10099 = AXIS2_PLACEMENT_3D('',#14677,#11731,#11732) ;
#10100 = AXIS2_PLACEMENT_3D('',#14682,#11734,#11735) ;
#10101 = AXIS2_PLACEMENT_3D('',#14703,#11737,#11738) ;
#10102 = AXIS2_PLACEMENT_3D('',#14704,#11739,#11740) ;
#10103 = AXIS2_PLACEMENT_3D('',#14706,#11741,#11742) ;
#10104 = AXIS2_PLACEMENT_3D('',#14709,#11744,#11745) ;
#10105 = AXIS2_PLACEMENT_3D('',#14710,#11746,#11747) ;
#10106 = AXIS2_PLACEMENT_3D('',#14711,#11748,#11749) ;
#10107 = AXIS2_PLACEMENT_3D('',#14731,#11751,#11752) ;
#10108 = AXIS2_PLACEMENT_3D('',#14732,#11753,#11754) ;
#10109 = AXIS2_PLACEMENT_3D('',#14733,#11755,#11756) ;
#10110 = AXIS2_PLACEMENT_3D('',#14734,#11757,#11758) ;
#10111 = AXIS2_PLACEMENT_3D('',#14736,#11759,#11760) ;
#10112 = AXIS2_PLACEMENT_3D('',#14737,#11761,#11762) ;
#10113 = AXIS2_PLACEMENT_3D('',#14738,#11763,#11764) ;
#10114 = AXIS2_PLACEMENT_3D('',#14739,#11765,#11766) ;
#10115 = AXIS2_PLACEMENT_3D('',#14740,#11767,#11768) ;
#10116 = AXIS2_PLACEMENT_3D('',#14742,#11769,#11770) ;
#10117 = AXIS2_PLACEMENT_3D('',#14744,#11772,#11773) ;
#10118 = AXIS2_PLACEMENT_3D('',#14746,#11774,#11775) ;
#10119 = AXIS2_PLACEMENT_3D('',#14747,#11776,#11777) ;
#10120 = AXIS2_PLACEMENT_3D('',#14749,#11778,#11779) ;
#10121 = AXIS2_PLACEMENT_3D('',#14751,#11781,#11782) ;
#10122 = AXIS2_PLACEMENT_3D('',#14752,#11783,#11784) ;
#10123 = AXIS2_PLACEMENT_3D('',#14753,#11785,#11786) ;
#10124 = AXIS2_PLACEMENT_3D('',#14758,#11788,#11789) ;
#10125 = AXIS2_PLACEMENT_3D('',#14761,#11791,#11792) ;
#10126 = AXIS2_PLACEMENT_3D('',#14762,#11793,#11794) ;
#10127 = AXIS2_PLACEMENT_3D('',#14780,#11802,#11803) ;
#10128 = AXIS2_PLACEMENT_3D('',#14784,#11806,#11807) ;
#10129 = AXIS2_PLACEMENT_3D('',#14788,#11810,#11811) ;
#10130 = AXIS2_PLACEMENT_3D('',#14791,#11812,#11813) ;
#10131 = AXIS2_PLACEMENT_3D('',#14795,#11816,#11817) ;
#10132 = AXIS2_PLACEMENT_3D('',#14796,#11818,#11819) ;
#10133 = AXIS2_PLACEMENT_3D('',#14798,#11821,#11822) ;
#10134 = AXIS2_PLACEMENT_3D('',#14809,#11827,#11828) ;
#10135 = AXIS2_PLACEMENT_3D('',#14811,#11830,#11831) ;
#10136 = AXIS2_PLACEMENT_3D('',#14812,#11832,#11833) ;
#10137 = AXIS2_PLACEMENT_3D('',#14813,#11834,#11835) ;
#10138 = AXIS2_PLACEMENT_3D('',#14814,#11836,#11837) ;
#10139 = AXIS2_PLACEMENT_3D('',#14816,#11838,#11839) ;
#10140 = AXIS2_PLACEMENT_3D('',#14817,#11840,#11841) ;
#10141 = AXIS2_PLACEMENT_3D('',#14818,#11842,#11843) ;
#10142 = AXIS2_PLACEMENT_3D('',#14822,#11845,#11846) ;
#10143 = AXIS2_PLACEMENT_3D('',#14823,#11847,#11848) ;
#10144 = AXIS2_PLACEMENT_3D('',#14827,#11850,#11851) ;
#10145 = AXIS2_PLACEMENT_3D('',#14831,#11854,#11855) ;
#10146 = AXIS2_PLACEMENT_3D('',#14832,#11856,#11857) ;
#10147 = AXIS2_PLACEMENT_3D('',#14842,#11863,#11864) ;
#10148 = AXIS2_PLACEMENT_3D('',#14848,#11868,#11869) ;
#10149 = AXIS2_PLACEMENT_3D('',#14852,#11872,#11873) ;
#10150 = AXIS2_PLACEMENT_3D('',#14856,#11876,#11877) ;
#10151 = AXIS2_PLACEMENT_3D('',#14858,#11879,#11880) ;
#10152 = AXIS2_PLACEMENT_3D('',#14859,#11881,#11882) ;
#10153 = AXIS2_PLACEMENT_3D('',#14860,#11883,#11884) ;
#10154 = AXIS2_PLACEMENT_3D('',#14869,#11889,#11890) ;
#10155 = AXIS2_PLACEMENT_3D('',#14875,#11894,#11895) ;
#10156 = AXIS2_PLACEMENT_3D('',#14881,#11899,#11900) ;
#10157 = AXIS2_PLACEMENT_3D('',#14891,#11906,#11907) ;
#10158 = AXIS2_PLACEMENT_3D('',#14893,#11909,#11910) ;
#10159 = AXIS2_PLACEMENT_3D('',#14897,#11912,#11913) ;
#10160 = AXIS2_PLACEMENT_3D('',#14900,#11915,#11916) ;
#10161 = AXIS2_PLACEMENT_3D('',#14902,#11917,#11918) ;
#10162 = AXIS2_PLACEMENT_3D('',#14903,#11919,#11920) ;
#10163 = AXIS2_PLACEMENT_3D('',#14907,#11923,#11924) ;
#10164 = AXIS2_PLACEMENT_3D('',#14910,#11926,#11927) ;
#10165 = AXIS2_PLACEMENT_3D('',#14911,#11928,#11929) ;
#10166 = AXIS2_PLACEMENT_3D('',#14914,#11931,#11932) ;
#10167 = AXIS2_PLACEMENT_3D('',#14915,#11933,#11934) ;
#10168 = AXIS2_PLACEMENT_3D('',#14919,#11937,#11938) ;
#10169 = AXIS2_PLACEMENT_3D('',#14920,#11939,#11940) ;
#10170 = AXIS2_PLACEMENT_3D('',#14921,#11941,#11942) ;
#10171 = AXIS2_PLACEMENT_3D('',#14922,#11943,#11944) ;
#10172 = AXIS2_PLACEMENT_3D('',#14923,#11945,#11946) ;
#10173 = AXIS2_PLACEMENT_3D('',#15003,#11948,#11949) ;
#10174 = AXIS2_PLACEMENT_3D('',#15083,#11951,#11952) ;
#10175 = AXIS2_PLACEMENT_3D('',#15085,#11953,#11954) ;
#10176 = AXIS2_PLACEMENT_3D('',#15088,#11956,#11957) ;
#10177 = AXIS2_PLACEMENT_3D('',#15089,#11958,#11959) ;
#10178 = AXIS2_PLACEMENT_3D('',#15092,#11960,#11961) ;
#10179 = AXIS2_PLACEMENT_3D('',#15102,#11967,#11968) ;
#10180 = AXIS2_PLACEMENT_3D('',#15108,#11972,#11973) ;
#10181 = AXIS2_PLACEMENT_3D('',#15114,#11977,#11978) ;
#10182 = AXIS2_PLACEMENT_3D('',#15118,#11981,#11982) ;
#10183 = AXIS2_PLACEMENT_3D('',#15120,#11984,#11985) ;
#10184 = AXIS2_PLACEMENT_3D('',#15124,#11988,#11989) ;
#10185 = AXIS2_PLACEMENT_3D('',#15125,#11990,#11991) ;
#10186 = AXIS2_PLACEMENT_3D('',#15126,#11992,#11993) ;
#10187 = AXIS2_PLACEMENT_3D('',#15128,#11994,#11995) ;
#10188 = AXIS2_PLACEMENT_3D('',#15133,#11998,#11999) ;
#10189 = AXIS2_PLACEMENT_3D('',#15134,#12000,#12001) ;
#10190 = AXIS2_PLACEMENT_3D('',#15135,#12002,#12003) ;
#10191 = AXIS2_PLACEMENT_3D('',#15137,#12004,#12005) ;
#10192 = AXIS2_PLACEMENT_3D('',#15139,#12006,#12007) ;
#10193 = AXIS2_PLACEMENT_3D('',#15140,#12008,#12009) ;
#10194 = AXIS2_PLACEMENT_3D('',#15141,#12010,#12011) ;
#10195 = AXIS2_PLACEMENT_3D('',#15145,#12013,#12014) ;
#10196 = AXIS2_PLACEMENT_3D('',#15146,#12015,#12016) ;
#10197 = AXIS2_PLACEMENT_3D('',#15147,#12017,#12018) ;
#10198 = AXIS2_PLACEMENT_3D('',#15149,#12019,#12020) ;
#10199 = AXIS2_PLACEMENT_3D('',#15151,#12021,#12022) ;
#10200 = AXIS2_PLACEMENT_3D('',#15152,#12023,#12024) ;
#10201 = AXIS2_PLACEMENT_3D('',#15153,#12025,#12026) ;
#10202 = AXIS2_PLACEMENT_3D('',#15157,#12029,#12030) ;
#10203 = AXIS2_PLACEMENT_3D('',#15158,#12031,#12032) ;
#10204 = AXIS2_PLACEMENT_3D('',#15159,#12033,#12034) ;
#10205 = AXIS2_PLACEMENT_3D('',#15160,#12035,#12036) ;
#10206 = AXIS2_PLACEMENT_3D('',#15161,#12037,#12038) ;
#10207 = AXIS2_PLACEMENT_3D('',#15163,#12039,#12040) ;
#10208 = AXIS2_PLACEMENT_3D('',#15166,#12042,#12043) ;
#10209 = AXIS2_PLACEMENT_3D('',#15167,#12044,#12045) ;
#10210 = AXIS2_PLACEMENT_3D('',#15176,#12050,#12051) ;
#10211 = AXIS2_PLACEMENT_3D('',#15178,#12052,#12053) ;
#10212 = AXIS2_PLACEMENT_3D('',#15180,#12054,#12055) ;
#10213 = AXIS2_PLACEMENT_3D('',#15182,#12057,#12058) ;
#10214 = AXIS2_PLACEMENT_3D('',#15188,#12062,#12063) ;
#10215 = AXIS2_PLACEMENT_3D('',#15189,#12064,#12065) ;
#10216 = AXIS2_PLACEMENT_3D('',#15190,#12066,#12067) ;
#10217 = AXIS2_PLACEMENT_3D('',#15191,#12068,#12069) ;
#10218 = AXIS2_PLACEMENT_3D('',#15192,#12070,#12071) ;
#10219 = AXIS2_PLACEMENT_3D('',#15193,#12072,#12073) ;
#10220 = AXIS2_PLACEMENT_3D('',#15194,#12074,#12075) ;
#10221 = AXIS2_PLACEMENT_3D('',#15196,#12076,#12077) ;
#10222 = AXIS2_PLACEMENT_3D('',#15197,#12078,#12079) ;
#10223 = AXIS2_PLACEMENT_3D('',#15199,#12080,#12081) ;
#10224 = AXIS2_PLACEMENT_3D('',#15201,#12083,#12084) ;
#10225 = AXIS2_PLACEMENT_3D('',#15203,#12085,#12086) ;
#10226 = AXIS2_PLACEMENT_3D('',#15205,#12088,#12089) ;
#10227 = AXIS2_PLACEMENT_3D('',#15207,#12090,#12091) ;
#10228 = AXIS2_PLACEMENT_3D('',#15208,#12092,#12093) ;
#10229 = AXIS2_PLACEMENT_3D('',#15210,#12094,#12095) ;
#10230 = AXIS2_PLACEMENT_3D('',#15212,#12097,#12098) ;
#10231 = AXIS2_PLACEMENT_3D('',#15214,#12099,#12100) ;
#10232 = AXIS2_PLACEMENT_3D('',#15215,#12101,#12102) ;
#10233 = AXIS2_PLACEMENT_3D('',#15217,#12103,#12104) ;
#10234 = AXIS2_PLACEMENT_3D('',#15219,#12106,#12107) ;
#10235 = AXIS2_PLACEMENT_3D('',#15221,#12108,#12109) ;
#10236 = AXIS2_PLACEMENT_3D('',#15222,#12110,#12111) ;
#10237 = AXIS2_PLACEMENT_3D('',#15224,#12112,#12113) ;
#10238 = AXIS2_PLACEMENT_3D('',#15226,#12115,#12116) ;
#10239 = AXIS2_PLACEMENT_3D('',#15228,#12117,#12118) ;
#10240 = AXIS2_PLACEMENT_3D('',#15230,#12120,#12121) ;
#10241 = AXIS2_PLACEMENT_3D('',#15231,#12122,#12123) ;
#10242 = AXIS2_PLACEMENT_3D('',#15232,#12124,#12125) ;
#10243 = AXIS2_PLACEMENT_3D('',#15241,#12130,#12131) ;
#10244 = AXIS2_PLACEMENT_3D('',#15250,#12136,#12137) ;
#10245 = AXIS2_PLACEMENT_3D('',#15256,#12141,#12142) ;
#10246 = AXIS2_PLACEMENT_3D('',#15262,#12146,#12147) ;
#10247 = AXIS2_PLACEMENT_3D('',#15263,#12148,#12149) ;
#10248 = AXIS2_PLACEMENT_3D('',#15264,#12150,#12151) ;
#10249 = AXIS2_PLACEMENT_3D('',#15265,#12152,#12153) ;
#10250 = AXIS2_PLACEMENT_3D('',#15266,#12154,#12155) ;
#10251 = AXIS2_PLACEMENT_3D('',#15267,#12156,#12157) ;
#10252 = AXIS2_PLACEMENT_3D('',#15268,#12158,#12159) ;
#10253 = AXIS2_PLACEMENT_3D('',#15269,#12160,#12161) ;
#10254 = AXIS2_PLACEMENT_3D('',#15270,#12162,#12163) ;
#10255 = AXIS2_PLACEMENT_3D('',#15271,#12164,#12165) ;
#10256 = AXIS2_PLACEMENT_3D('',#15273,#12166,#12167) ;
#10257 = AXIS2_PLACEMENT_3D('',#15274,#12168,#12169) ;
#10258 = AXIS2_PLACEMENT_3D('',#15276,#12170,#12171) ;
#10259 = AXIS2_PLACEMENT_3D('',#15278,#12173,#12174) ;
#10260 = AXIS2_PLACEMENT_3D('',#15280,#12175,#12176) ;
#10261 = AXIS2_PLACEMENT_3D('',#15282,#12178,#12179) ;
#10262 = AXIS2_PLACEMENT_3D('',#15284,#12180,#12181) ;
#10263 = AXIS2_PLACEMENT_3D('',#15286,#12183,#12184) ;
#10264 = AXIS2_PLACEMENT_3D('',#15288,#12185,#12186) ;
#10265 = AXIS2_PLACEMENT_3D('',#15289,#12187,#12188) ;
#10266 = AXIS2_PLACEMENT_3D('',#15291,#12189,#12190) ;
#10267 = AXIS2_PLACEMENT_3D('',#15293,#12192,#12193) ;
#10268 = AXIS2_PLACEMENT_3D('',#15295,#12194,#12195) ;
#10269 = AXIS2_PLACEMENT_3D('',#15297,#12197,#12198) ;
#10270 = AXIS2_PLACEMENT_3D('',#15298,#12199,#12200) ;
#10271 = AXIS2_PLACEMENT_3D('',#15299,#12201,#12202) ;
#10272 = AXIS2_PLACEMENT_3D('',#15315,#12204,#12205) ;
#10273 = AXIS2_PLACEMENT_3D('',#15323,#12206,#12207) ;
#10274 = AXIS2_PLACEMENT_3D('',#15371,#12209,#12210) ;
#10275 = AXIS2_PLACEMENT_3D('',#15419,#12212,#12213) ;
#10276 = AXIS2_PLACEMENT_3D('',#15473,#12215,#12216) ;
#10277 = AXIS2_PLACEMENT_3D('',#15521,#12218,#12219) ;
#10278 = AXIS2_PLACEMENT_3D('',#15569,#12221,#12222) ;
#10279 = AXIS2_PLACEMENT_3D('',#15623,#12224,#12225) ;
#10280 = AXIS2_PLACEMENT_3D('',#15671,#12227,#12228) ;
#10281 = AXIS2_PLACEMENT_3D('',#15719,#12230,#12231) ;
#10282 = AXIS2_PLACEMENT_3D('',#15773,#12233,#12234) ;
#10283 = AXIS2_PLACEMENT_3D('',#15821,#12236,#12237) ;
#10284 = AXIS2_PLACEMENT_3D('',#15869,#12239,#12240) ;
#10285 = AXIS2_PLACEMENT_3D('',#15923,#12242,#12243) ;
#10286 = AXIS2_PLACEMENT_3D('',#15971,#12245,#12246) ;
#10287 = AXIS2_PLACEMENT_3D('',#15982,#12248,#12249) ;
#10288 = AXIS2_PLACEMENT_3D('',#15987,#12250,#12251) ;
#10289 = AXIS2_PLACEMENT_3D('',#16011,#12253,#12254) ;
#10290 = AXIS2_PLACEMENT_3D('',#16036,#12256,#12257) ;
#10291 = AXIS2_PLACEMENT_3D('',#16061,#12259,#12260) ;
#10292 = AXIS2_PLACEMENT_3D('',#16085,#12262,#12263) ;
#10293 = AXIS2_PLACEMENT_3D('',#16110,#12265,#12266) ;
#10294 = AXIS2_PLACEMENT_3D('',#16135,#12268,#12269) ;
#10295 = AXIS2_PLACEMENT_3D('',#16159,#12271,#12272) ;
#10296 = AXIS2_PLACEMENT_3D('',#16184,#12274,#12275) ;
#10297 = AXIS2_PLACEMENT_3D('',#16209,#12277,#12278) ;
#10298 = AXIS2_PLACEMENT_3D('',#16233,#12280,#12281) ;
#10299 = AXIS2_PLACEMENT_3D('',#16258,#12283,#12284) ;
#10300 = AXIS2_PLACEMENT_3D('',#16283,#12286,#12287) ;
#10301 = AXIS2_PLACEMENT_3D('',#16307,#12289,#12290) ;
#10302 = AXIS2_PLACEMENT_3D('',#16383,#12291,#12292) ;
#10303 = AXIS2_PLACEMENT_3D('',#16385,#12293,#12294) ;
#10304 = AXIS2_PLACEMENT_3D('',#16933,#12295,#12296) ;
#10305 = AXIS2_PLACEMENT_3D('',#16935,#12297,#12298) ;
#10306 = AXIS2_PLACEMENT_3D('',#17013,#12299,#12300) ;
#10307 = AXIS2_PLACEMENT_3D('',#17014,#12301,#12302) ;
#10308 = AXIS2_PLACEMENT_3D('',#17015,#12303,#12304) ;
#10309 = AXIS2_PLACEMENT_3D('',#17409,#12305,#12306) ;
#10310 = AXIS2_PLACEMENT_3D('',#17411,#12307,#12308) ;
#10311 = AXIS2_PLACEMENT_3D('',#17412,#12309,#12310) ;
#10312 = AXIS2_PLACEMENT_3D('',#17413,#12311,#12312) ;
#10313 = AXIS2_PLACEMENT_3D('',#17414,#12313,#12314) ;
#10314 = AXIS2_PLACEMENT_3D('',#17415,#12315,#12316) ;
#10315 = AXIS2_PLACEMENT_3D('',#17417,#12317,#12318) ;
#10316 = AXIS2_PLACEMENT_3D('',#17418,#12319,#12320) ;
#10317 = AXIS2_PLACEMENT_3D('',#17421,#12322,#12323) ;
#10318 = AXIS2_PLACEMENT_3D('',#17422,#12324,#12325) ;
#10319 = AXIS2_PLACEMENT_3D('',#17423,#12326,#12327) ;
#10320 = AXIS2_PLACEMENT_3D('',#17426,#12328,#12329) ;
#10321 = AXIS2_PLACEMENT_3D('',#17430,#12332,#12333) ;
#10322 = AXIS2_PLACEMENT_3D('',#17438,#12336,#12337) ;
#10323 = AXIS2_PLACEMENT_3D('',#17444,#12339,#12340) ;
#10324 = AXIS2_PLACEMENT_3D('',#17446,#12341,#12342) ;
#10325 = AXIS2_PLACEMENT_3D('',#17450,#12344,#12345) ;
#10326 = AXIS2_PLACEMENT_3D('',#17454,#12347,#12348) ;
#10327 = AXIS2_PLACEMENT_3D('',#17458,#12350,#12351) ;
#10328 = AXIS2_PLACEMENT_3D('',#17462,#12353,#12354) ;
#10329 = AXIS2_PLACEMENT_3D('',#17466,#12356,#12357) ;
#10330 = AXIS2_PLACEMENT_3D('',#17470,#12359,#12360) ;
#10331 = AXIS2_PLACEMENT_3D('',#17474,#12362,#12363) ;
#10332 = AXIS2_PLACEMENT_3D('',#17478,#12365,#12366) ;
#10333 = AXIS2_PLACEMENT_3D('',#17482,#12368,#12369) ;
#10334 = AXIS2_PLACEMENT_3D('',#17486,#12371,#12372) ;
#10335 = AXIS2_PLACEMENT_3D('',#17490,#12374,#12375) ;
#10336 = AXIS2_PLACEMENT_3D('',#17494,#12377,#12378) ;
#10337 = AXIS2_PLACEMENT_3D('',#17498,#12380,#12381) ;
#10338 = AXIS2_PLACEMENT_3D('',#17502,#12383,#12384) ;
#10339 = AXIS2_PLACEMENT_3D('',#17506,#12386,#12387) ;
#10340 = AXIS2_PLACEMENT_3D('',#17510,#12389,#12390) ;
#10341 = AXIS2_PLACEMENT_3D('',#17514,#12392,#12393) ;
#10342 = AXIS2_PLACEMENT_3D('',#17518,#12395,#12396) ;
#10343 = AXIS2_PLACEMENT_3D('',#17522,#12398,#12399) ;
#10344 = AXIS2_PLACEMENT_3D('',#17526,#12401,#12402) ;
#10345 = AXIS2_PLACEMENT_3D('',#17530,#12404,#12405) ;
#10346 = AXIS2_PLACEMENT_3D('',#17534,#12407,#12408) ;
#10347 = AXIS2_PLACEMENT_3D('',#17538,#12410,#12411) ;
#10348 = AXIS2_PLACEMENT_3D('',#17542,#12413,#12414) ;
#10349 = AXIS2_PLACEMENT_3D('',#17546,#12416,#12417) ;
#10350 = AXIS2_PLACEMENT_3D('',#17550,#12419,#12420) ;
#10351 = AXIS2_PLACEMENT_3D('',#17554,#12422,#12423) ;
#10352 = AXIS2_PLACEMENT_3D('',#17558,#12425,#12426) ;
#10353 = AXIS2_PLACEMENT_3D('',#17562,#12428,#12429) ;
#10354 = AXIS2_PLACEMENT_3D('',#17566,#12431,#12432) ;
#10355 = AXIS2_PLACEMENT_3D('',#17570,#12434,#12435) ;
#10356 = AXIS2_PLACEMENT_3D('',#17574,#12437,#12438) ;
#10357 = AXIS2_PLACEMENT_3D('',#17578,#12440,#12441) ;
#10358 = AXIS2_PLACEMENT_3D('',#17582,#12443,#12444) ;
#10359 = AXIS2_PLACEMENT_3D('',#17586,#12446,#12447) ;
#10360 = AXIS2_PLACEMENT_3D('',#17590,#12449,#12450) ;
#10361 = AXIS2_PLACEMENT_3D('',#17594,#12452,#12453) ;
#10362 = AXIS2_PLACEMENT_3D('',#17597,#12455,#12456) ;
#10363 = AXIS2_PLACEMENT_3D('',#17599,#12457,#12458) ;
#10364 = AXIS2_PLACEMENT_3D('',#17603,#12460,#12461) ;
#10365 = AXIS2_PLACEMENT_3D('',#17607,#12463,#12464) ;
#10366 = AXIS2_PLACEMENT_3D('',#17611,#12466,#12467) ;
#10367 = AXIS2_PLACEMENT_3D('',#17615,#12469,#12470) ;
#10368 = AXIS2_PLACEMENT_3D('',#17619,#12472,#12473) ;
#10369 = AXIS2_PLACEMENT_3D('',#17623,#12475,#12476) ;
#10370 = AXIS2_PLACEMENT_3D('',#17627,#12478,#12479) ;
#10371 = AXIS2_PLACEMENT_3D('',#17631,#12481,#12482) ;
#10372 = AXIS2_PLACEMENT_3D('',#17635,#12484,#12485) ;
#10373 = AXIS2_PLACEMENT_3D('',#17639,#12487,#12488) ;
#10374 = AXIS2_PLACEMENT_3D('',#17643,#12490,#12491) ;
#10375 = AXIS2_PLACEMENT_3D('',#17647,#12493,#12494) ;
#10376 = AXIS2_PLACEMENT_3D('',#17651,#12496,#12497) ;
#10377 = AXIS2_PLACEMENT_3D('',#17655,#12499,#12500) ;
#10378 = AXIS2_PLACEMENT_3D('',#17659,#12502,#12503) ;
#10379 = AXIS2_PLACEMENT_3D('',#17663,#12505,#12506) ;
#10380 = AXIS2_PLACEMENT_3D('',#17667,#12508,#12509) ;
#10381 = AXIS2_PLACEMENT_3D('',#17671,#12511,#12512) ;
#10382 = AXIS2_PLACEMENT_3D('',#17675,#12514,#12515) ;
#10383 = AXIS2_PLACEMENT_3D('',#17679,#12517,#12518) ;
#10384 = AXIS2_PLACEMENT_3D('',#17683,#12520,#12521) ;
#10385 = AXIS2_PLACEMENT_3D('',#17687,#12523,#12524) ;
#10386 = AXIS2_PLACEMENT_3D('',#17691,#12526,#12527) ;
#10387 = AXIS2_PLACEMENT_3D('',#17695,#12529,#12530) ;
#10388 = AXIS2_PLACEMENT_3D('',#17699,#12532,#12533) ;
#10389 = AXIS2_PLACEMENT_3D('',#17703,#12535,#12536) ;
#10390 = AXIS2_PLACEMENT_3D('',#17707,#12538,#12539) ;
#10391 = AXIS2_PLACEMENT_3D('',#17711,#12541,#12542) ;
#10392 = AXIS2_PLACEMENT_3D('',#17715,#12544,#12545) ;
#10393 = AXIS2_PLACEMENT_3D('',#17719,#12547,#12548) ;
#10394 = AXIS2_PLACEMENT_3D('',#17723,#12550,#12551) ;
#10395 = AXIS2_PLACEMENT_3D('',#17727,#12553,#12554) ;
#10396 = AXIS2_PLACEMENT_3D('',#17730,#12556,#12557) ;
#10397 = AXIS2_PLACEMENT_3D('',#17731,#12558,#12559) ;
#10398 = AXIS2_PLACEMENT_3D('',#17739,#12562,#12563) ;
#10399 = AXIS2_PLACEMENT_3D('',#17744,#12565,#12566) ;
#10400 = AXIS2_PLACEMENT_3D('',#17745,#12567,#12568) ;
#10401 = AXIS2_PLACEMENT_3D('',#17747,#12569,#12570) ;
#10402 = AXIS2_PLACEMENT_3D('',#17987,#12572,#12573) ;
#10403 = AXIS2_PLACEMENT_3D('',#17991,#12576,#12577) ;
#10404 = AXIS2_PLACEMENT_3D('',#17993,#12579,#12580) ;
#10405 = AXIS2_PLACEMENT_3D('',#17994,#12581,#12582) ;
#10406 = AXIS2_PLACEMENT_3D('',#17998,#12585,#12586) ;
#10407 = AXIS2_PLACEMENT_3D('',#18000,#12588,#12589) ;
#10408 = AXIS2_PLACEMENT_3D('',#18001,#12590,#12591) ;
#10409 = AXIS2_PLACEMENT_3D('',#18005,#12594,#12595) ;
#10410 = AXIS2_PLACEMENT_3D('',#18007,#12597,#12598) ;
#10411 = AXIS2_PLACEMENT_3D('',#18008,#12599,#12600) ;
#10412 = AXIS2_PLACEMENT_3D('',#18012,#12603,#12604) ;
#10413 = AXIS2_PLACEMENT_3D('',#18014,#12606,#12607) ;
#10414 = AXIS2_PLACEMENT_3D('',#18015,#12608,#12609) ;
#10415 = AXIS2_PLACEMENT_3D('',#18019,#12612,#12613) ;
#10416 = AXIS2_PLACEMENT_3D('',#18021,#12615,#12616) ;
#10417 = AXIS2_PLACEMENT_3D('',#18022,#12617,#12618) ;
#10418 = AXIS2_PLACEMENT_3D('',#18026,#12621,#12622) ;
#10419 = AXIS2_PLACEMENT_3D('',#18028,#12624,#12625) ;
#10420 = AXIS2_PLACEMENT_3D('',#18029,#12626,#12627) ;
#10421 = AXIS2_PLACEMENT_3D('',#18033,#12630,#12631) ;
#10422 = AXIS2_PLACEMENT_3D('',#18035,#12633,#12634) ;
#10423 = AXIS2_PLACEMENT_3D('',#18036,#12635,#12636) ;
#10424 = AXIS2_PLACEMENT_3D('',#18040,#12639,#12640) ;
#10425 = AXIS2_PLACEMENT_3D('',#18042,#12642,#12643) ;
#10426 = AXIS2_PLACEMENT_3D('',#18043,#12644,#12645) ;
#10427 = AXIS2_PLACEMENT_3D('',#18047,#12648,#12649) ;
#10428 = AXIS2_PLACEMENT_3D('',#18049,#12651,#12652) ;
#10429 = AXIS2_PLACEMENT_3D('',#18050,#12653,#12654) ;
#10430 = AXIS2_PLACEMENT_3D('',#18054,#12657,#12658) ;
#10431 = AXIS2_PLACEMENT_3D('',#18056,#12660,#12661) ;
#10432 = AXIS2_PLACEMENT_3D('',#18057,#12662,#12663) ;
#10433 = AXIS2_PLACEMENT_3D('',#18061,#12666,#12667) ;
#10434 = AXIS2_PLACEMENT_3D('',#18063,#12669,#12670) ;
#10435 = AXIS2_PLACEMENT_3D('',#18064,#12671,#12672) ;
#10436 = AXIS2_PLACEMENT_3D('',#18068,#12675,#12676) ;
#10437 = AXIS2_PLACEMENT_3D('',#18070,#12678,#12679) ;
#10438 = AXIS2_PLACEMENT_3D('',#18071,#12680,#12681) ;
#10439 = AXIS2_PLACEMENT_3D('',#18075,#12684,#12685) ;
#10440 = AXIS2_PLACEMENT_3D('',#18077,#12687,#12688) ;
#10441 = AXIS2_PLACEMENT_3D('',#18078,#12689,#12690) ;
#10442 = AXIS2_PLACEMENT_3D('',#18082,#12693,#12694) ;
#10443 = AXIS2_PLACEMENT_3D('',#18084,#12696,#12697) ;
#10444 = AXIS2_PLACEMENT_3D('',#18085,#12698,#12699) ;
#10445 = AXIS2_PLACEMENT_3D('',#18089,#12702,#12703) ;
#10446 = AXIS2_PLACEMENT_3D('',#18091,#12705,#12706) ;
#10447 = AXIS2_PLACEMENT_3D('',#18092,#12707,#12708) ;
#10448 = AXIS2_PLACEMENT_3D('',#18096,#12711,#12712) ;
#10449 = AXIS2_PLACEMENT_3D('',#18098,#12714,#12715) ;
#10450 = AXIS2_PLACEMENT_3D('',#18099,#12716,#12717) ;
#10451 = AXIS2_PLACEMENT_3D('',#18103,#12720,#12721) ;
#10452 = AXIS2_PLACEMENT_3D('',#18105,#12723,#12724) ;
#10453 = AXIS2_PLACEMENT_3D('',#18106,#12725,#12726) ;
#10454 = AXIS2_PLACEMENT_3D('',#18110,#12729,#12730) ;
#10455 = AXIS2_PLACEMENT_3D('',#18112,#12732,#12733) ;
#10456 = AXIS2_PLACEMENT_3D('',#18113,#12734,#12735) ;
#10457 = AXIS2_PLACEMENT_3D('',#18117,#12738,#12739) ;
#10458 = AXIS2_PLACEMENT_3D('',#18119,#12741,#12742) ;
#10459 = AXIS2_PLACEMENT_3D('',#18120,#12743,#12744) ;
#10460 = AXIS2_PLACEMENT_3D('',#18124,#12747,#12748) ;
#10461 = AXIS2_PLACEMENT_3D('',#18126,#12750,#12751) ;
#10462 = AXIS2_PLACEMENT_3D('',#18127,#12752,#12753) ;
#10463 = AXIS2_PLACEMENT_3D('',#18131,#12756,#12757) ;
#10464 = AXIS2_PLACEMENT_3D('',#18133,#12759,#12760) ;
#10465 = AXIS2_PLACEMENT_3D('',#18134,#12761,#12762) ;
#10466 = AXIS2_PLACEMENT_3D('',#18138,#12765,#12766) ;
#10467 = AXIS2_PLACEMENT_3D('',#18140,#12768,#12769) ;
#10468 = AXIS2_PLACEMENT_3D('',#18141,#12770,#12771) ;
#10469 = AXIS2_PLACEMENT_3D('',#18145,#12774,#12775) ;
#10470 = AXIS2_PLACEMENT_3D('',#18147,#12777,#12778) ;
#10471 = AXIS2_PLACEMENT_3D('',#18148,#12779,#12780) ;
#10472 = AXIS2_PLACEMENT_3D('',#18152,#12783,#12784) ;
#10473 = AXIS2_PLACEMENT_3D('',#18154,#12786,#12787) ;
#10474 = AXIS2_PLACEMENT_3D('',#18155,#12788,#12789) ;
#10475 = AXIS2_PLACEMENT_3D('',#18159,#12792,#12793) ;
#10476 = AXIS2_PLACEMENT_3D('',#18161,#12795,#12796) ;
#10477 = AXIS2_PLACEMENT_3D('',#18162,#12797,#12798) ;
#10478 = AXIS2_PLACEMENT_3D('',#18166,#12801,#12802) ;
#10479 = AXIS2_PLACEMENT_3D('',#18168,#12804,#12805) ;
#10480 = AXIS2_PLACEMENT_3D('',#18169,#12806,#12807) ;
#10481 = AXIS2_PLACEMENT_3D('',#18173,#12810,#12811) ;
#10482 = AXIS2_PLACEMENT_3D('',#18175,#12813,#12814) ;
#10483 = AXIS2_PLACEMENT_3D('',#18176,#12815,#12816) ;
#10484 = AXIS2_PLACEMENT_3D('',#18180,#12819,#12820) ;
#10485 = AXIS2_PLACEMENT_3D('',#18182,#12822,#12823) ;
#10486 = AXIS2_PLACEMENT_3D('',#18183,#12824,#12825) ;
#10487 = AXIS2_PLACEMENT_3D('',#18187,#12828,#12829) ;
#10488 = AXIS2_PLACEMENT_3D('',#18189,#12831,#12832) ;
#10489 = AXIS2_PLACEMENT_3D('',#18190,#12833,#12834) ;
#10490 = AXIS2_PLACEMENT_3D('',#18194,#12837,#12838) ;
#10491 = AXIS2_PLACEMENT_3D('',#18196,#12840,#12841) ;
#10492 = AXIS2_PLACEMENT_3D('',#18197,#12842,#12843) ;
#10493 = AXIS2_PLACEMENT_3D('',#18201,#12846,#12847) ;
#10494 = AXIS2_PLACEMENT_3D('',#18203,#12849,#12850) ;
#10495 = AXIS2_PLACEMENT_3D('',#18204,#12851,#12852) ;
#10496 = AXIS2_PLACEMENT_3D('',#18208,#12855,#12856) ;
#10497 = AXIS2_PLACEMENT_3D('',#18210,#12858,#12859) ;
#10498 = AXIS2_PLACEMENT_3D('',#18211,#12860,#12861) ;
#10499 = AXIS2_PLACEMENT_3D('',#18215,#12864,#12865) ;
#10500 = AXIS2_PLACEMENT_3D('',#18217,#12867,#12868) ;
#10501 = AXIS2_PLACEMENT_3D('',#18218,#12869,#12870) ;
#10502 = AXIS2_PLACEMENT_3D('',#18222,#12873,#12874) ;
#10503 = AXIS2_PLACEMENT_3D('',#18224,#12876,#12877) ;
#10504 = AXIS2_PLACEMENT_3D('',#18225,#12878,#12879) ;
#10505 = AXIS2_PLACEMENT_3D('',#18226,#12880,#12881) ;
#10506 = AXIS2_PLACEMENT_3D('',#18227,#12882,#12883) ;
#10507 = AXIS2_PLACEMENT_3D('',#18229,#12884,#12885) ;
#10508 = AXIS2_PLACEMENT_3D('',#18230,#12886,#12887) ;
#10509 = AXIS2_PLACEMENT_3D('',#18238,#12889,#12890) ;
#10510 = AXIS2_PLACEMENT_3D('',#18248,#12891,#12892) ;
#10511 = AXIS2_PLACEMENT_3D('',#18258,#12893,#12894) ;
#10512 = AXIS2_PLACEMENT_3D('',#18268,#12895,#12896) ;
#10513 = AXIS2_PLACEMENT_3D('',#18278,#12897,#12898) ;
#10514 = AXIS2_PLACEMENT_3D('',#18288,#12899,#12900) ;
#10515 = AXIS2_PLACEMENT_3D('',#18292,#12901,#12902) ;
#10516 = AXIS2_PLACEMENT_3D('',#18297,#12905,#12906) ;
#10517 = AXIS2_PLACEMENT_3D('',#18298,#12907,#12908) ;
#10518 = AXIS2_PLACEMENT_3D('',#18303,#12911,#12912) ;
#10519 = AXIS2_PLACEMENT_3D('',#18304,#12913,#12914) ;
#10520 = AXIS2_PLACEMENT_3D('',#18308,#12916,#12917) ;
#10521 = AXIS2_PLACEMENT_3D('',#18310,#12919,#12920) ;
#10522 = AXIS2_PLACEMENT_3D('',#18315,#12923,#12924) ;
#10523 = AXIS2_PLACEMENT_3D('',#18316,#12925,#12926) ;
#10524 = AXIS2_PLACEMENT_3D('',#18320,#12928,#12929) ;
#10525 = AXIS2_PLACEMENT_3D('',#18322,#12931,#12932) ;
#10526 = AXIS2_PLACEMENT_3D('',#18326,#12934,#12935) ;
#10527 = AXIS2_PLACEMENT_3D('',#18328,#12937,#12938) ;
#10528 = AXIS2_PLACEMENT_3D('',#18335,#12943,#12944) ;
#10529 = AXIS2_PLACEMENT_3D('',#18340,#12948,#12949) ;
#10530 = AXIS2_PLACEMENT_3D('',#18345,#12953,#12954) ;
#10531 = AXIS2_PLACEMENT_3D('',#18346,#12955,#12956) ;
#10532 = AXIS2_PLACEMENT_3D('',#18347,#12957,#12958) ;
#10533 = AXIS2_PLACEMENT_3D('',#18349,#12960,#12961) ;
#10534 = AXIS2_PLACEMENT_3D('',#18350,#12962,#12963) ;
#10535 = AXIS2_PLACEMENT_3D('',#18352,#12965,#12966) ;
#10536 = AXIS2_PLACEMENT_3D('',#18354,#12968,#12969) ;
#10537 = AXIS2_PLACEMENT_3D('',#18357,#12971,#12972) ;
#10538 = AXIS2_PLACEMENT_3D('',#18358,#12973,#12974) ;
#10539 = AXIS2_PLACEMENT_3D('',#18359,#12975,#12976) ;
#10540 = AXIS2_PLACEMENT_3D('',#18360,#12977,#12978) ;
#10541 = AXIS2_PLACEMENT_3D('',#18361,#12979,#12980) ;
#10542 = AXIS2_PLACEMENT_3D('',#18362,#12981,#12982) ;
#10543 = AXIS2_PLACEMENT_3D('',#18363,#12983,#12984) ;
#10544 = AXIS2_PLACEMENT_3D('',#18364,#12985,#12986) ;
#10545 = AXIS2_PLACEMENT_3D('',#18367,#12988,#12989) ;
#10546 = AXIS2_PLACEMENT_3D('',#18368,#12990,#12991) ;
#10547 = AXIS2_PLACEMENT_3D('',#18370,#12993,#12994) ;
#10548 = AXIS2_PLACEMENT_3D('',#18371,#12995,#12996) ;
#10549 = AXIS2_PLACEMENT_3D('',#18374,#12998,#12999) ;
#10550 = AXIS2_PLACEMENT_3D('',#18376,#13001,#13002) ;
#10551 = AXIS2_PLACEMENT_3D('',#18378,#13004,#13005) ;
#10552 = AXIS2_PLACEMENT_3D('',#18379,#13006,#13007) ;
#10553 = AXIS2_PLACEMENT_3D('',#18380,#13008,#13009) ;
#10554 = AXIS2_PLACEMENT_3D('',#18382,#13010,#13011) ;
#10555 = AXIS2_PLACEMENT_3D('',#18385,#13013,#13014) ;
#10556 = AXIS2_PLACEMENT_3D('',#18386,#13015,#13016) ;
#10557 = AXIS2_PLACEMENT_3D('',#18388,#13017,#13018) ;
#10558 = AXIS2_PLACEMENT_3D('',#18391,#13020,#13021) ;
#10559 = AXIS2_PLACEMENT_3D('',#18392,#13022,#13023) ;
#10560 = AXIS2_PLACEMENT_3D('',#18395,#13024,#13025) ;
#10561 = AXIS2_PLACEMENT_3D('',#18405,#13031,#13032) ;
#10562 = AXIS2_PLACEMENT_3D('',#18407,#13033,#13034) ;
#10563 = AXIS2_PLACEMENT_3D('',#18410,#13036,#13037) ;
#10564 = AXIS2_PLACEMENT_3D('',#18411,#13038,#13039) ;
#10565 = AXIS2_PLACEMENT_3D('',#18417,#13043,#13044) ;
#10566 = AXIS2_PLACEMENT_3D('',#18419,#13045,#13046) ;
#10567 = AXIS2_PLACEMENT_3D('',#18421,#13047,#13048) ;
#10568 = AXIS2_PLACEMENT_3D('',#18423,#13050,#13051) ;
#10569 = AXIS2_PLACEMENT_3D('',#18426,#13054,#13055) ;
#10570 = AXIS2_PLACEMENT_3D('',#18432,#13059,#13060) ;
#10571 = AXIS2_PLACEMENT_3D('',#18433,#13061,#13062) ;
#10572 = AXIS2_PLACEMENT_3D('',#18435,#13063,#13064) ;
#10573 = AXIS2_PLACEMENT_3D('',#18437,#13065,#13066) ;
#10574 = AXIS2_PLACEMENT_3D('',#18440,#13068,#13069) ;
#10575 = AXIS2_PLACEMENT_3D('',#18441,#13070,#13071) ;
#10576 = AXIS2_PLACEMENT_3D('',#18451,#13076,#13077) ;
#10577 = AXIS2_PLACEMENT_3D('',#18456,#13080,#13081) ;
#10578 = AXIS2_PLACEMENT_3D('',#18457,#13082,#13083) ;
#10579 = AXIS2_PLACEMENT_3D('',#18459,#13084,#13085) ;
#10580 = AXIS2_PLACEMENT_3D('',#18461,#13087,#13088) ;
#10581 = AXIS2_PLACEMENT_3D('',#18467,#13092,#13093) ;
#10582 = AXIS2_PLACEMENT_3D('',#18469,#13094,#13095) ;
#10583 = AXIS2_PLACEMENT_3D('',#18471,#13097,#13098) ;
#10584 = AXIS2_PLACEMENT_3D('',#18475,#13101,#13102) ;
#10585 = AXIS2_PLACEMENT_3D('',#18476,#13103,#13104) ;
#10586 = AXIS2_PLACEMENT_3D('',#18478,#13106,#13107) ;
#10587 = AXIS2_PLACEMENT_3D('',#18479,#13108,#13109) ;
#10588 = AXIS2_PLACEMENT_3D('',#18481,#13110,#13111) ;
#10589 = AXIS2_PLACEMENT_3D('',#18483,#13113,#13114) ;
#10590 = AXIS2_PLACEMENT_3D('',#18485,#13115,#13116) ;
#10591 = AXIS2_PLACEMENT_3D('',#18486,#13117,#13118) ;
#10592 = AXIS2_PLACEMENT_3D('',#18489,#13120,#13121) ;
#10593 = AXIS2_PLACEMENT_3D('',#18490,#13122,#13123) ;
#10594 = AXIS2_PLACEMENT_3D('',#18499,#13128,#13129) ;
#10595 = AXIS2_PLACEMENT_3D('',#18505,#13133,#13134) ;
#10596 = AXIS2_PLACEMENT_3D('',#18511,#13138,#13139) ;
#10597 = AXIS2_PLACEMENT_3D('',#18514,#13142,#13143) ;
#10598 = AXIS2_PLACEMENT_3D('',#18515,#13144,#13145) ;
#10599 = AXIS2_PLACEMENT_3D('',#18516,#13146,#13147) ;
#10600 = AXIS2_PLACEMENT_3D('',#18517,#13148,#13149) ;
#10601 = AXIS2_PLACEMENT_3D('',#18519,#13150,#13151) ;
#10602 = AXIS2_PLACEMENT_3D('',#18522,#13153,#13154) ;
#10603 = AXIS2_PLACEMENT_3D('',#18523,#13155,#13156) ;
#10604 = AXIS2_PLACEMENT_3D('',#18525,#13157,#13158) ;
#10605 = AXIS2_PLACEMENT_3D('',#18528,#13160,#13161) ;
#10606 = AXIS2_PLACEMENT_3D('',#18529,#13162,#13163) ;
#10607 = AXIS2_PLACEMENT_3D('',#18536,#13166,#13167) ;
#10608 = AXIS2_PLACEMENT_3D('',#18539,#13169,#13170) ;
#10609 = AXIS2_PLACEMENT_3D('',#18540,#13171,#13172) ;
#10610 = AXIS2_PLACEMENT_3D('',#18546,#13176,#13177) ;
#10611 = AXIS2_PLACEMENT_3D('',#18549,#13179,#13180) ;
#10612 = AXIS2_PLACEMENT_3D('',#18550,#13181,#13182) ;
#10613 = AXIS2_PLACEMENT_3D('',#18556,#13186,#13187) ;
#10614 = AXIS2_PLACEMENT_3D('',#18557,#13188,#13189) ;
#10615 = AXIS2_PLACEMENT_3D('',#18558,#13190,#13191) ;
#10616 = AXIS2_PLACEMENT_3D('',#18560,#13193,#13194) ;
#10617 = AXIS2_PLACEMENT_3D('',#18567,#13197,#13198) ;
#10618 = AXIS2_PLACEMENT_3D('',#18570,#13200,#13201) ;
#10619 = AXIS2_PLACEMENT_3D('',#18571,#13202,#13203) ;
#10620 = AXIS2_PLACEMENT_3D('',#18577,#13207,#13208) ;
#10621 = AXIS2_PLACEMENT_3D('',#18580,#13210,#13211) ;
#10622 = AXIS2_PLACEMENT_3D('',#18581,#13212,#13213) ;
#10623 = AXIS2_PLACEMENT_3D('',#18587,#13217,#13218) ;
#10624 = AXIS2_PLACEMENT_3D('',#18588,#13219,#13220) ;
#10625 = AXIS2_PLACEMENT_3D('',#18589,#13221,#13222) ;
#10626 = AXIS2_PLACEMENT_3D('',#18591,#13224,#13225) ;
#10627 = AXIS2_PLACEMENT_3D('',#18600,#13230,#13231) ;
#10628 = AXIS2_PLACEMENT_3D('',#18606,#13235,#13236) ;
#10629 = AXIS2_PLACEMENT_3D('',#18612,#13240,#13241) ;
#10630 = AXIS2_PLACEMENT_3D('',#18615,#13244,#13245) ;
#10631 = AXIS2_PLACEMENT_3D('',#18616,#13246,#13247) ;
#10632 = AXIS2_PLACEMENT_3D('',#18617,#13248,#13249) ;
#10633 = AXIS2_PLACEMENT_3D('',#18618,#13250,#13251) ;
#10634 = AXIS2_PLACEMENT_3D('',#18620,#13252,#13253) ;
#10635 = AXIS2_PLACEMENT_3D('',#18622,#13254,#13255) ;
#10636 = AXIS2_PLACEMENT_3D('',#18623,#13256,#13257) ;
#10637 = AXIS2_PLACEMENT_3D('',#18625,#13258,#13259) ;
#10638 = AXIS2_PLACEMENT_3D('',#18627,#13261,#13262) ;
#10639 = AXIS2_PLACEMENT_3D('',#18629,#13263,#13264) ;
#10640 = AXIS2_PLACEMENT_3D('',#18630,#13265,#13266) ;
#10641 = AXIS2_PLACEMENT_3D('',#18632,#13267,#13268) ;
#10642 = AXIS2_PLACEMENT_3D('',#18634,#13270,#13271) ;
#10643 = AXIS2_PLACEMENT_3D('',#18636,#13272,#13273) ;
#10644 = AXIS2_PLACEMENT_3D('',#18638,#13275,#13276) ;
#10645 = AXIS2_PLACEMENT_3D('',#18640,#13277,#13278) ;
#10646 = AXIS2_PLACEMENT_3D('',#18642,#13280,#13281) ;
#10647 = AXIS2_PLACEMENT_3D('',#18644,#13282,#13283) ;
#10648 = AXIS2_PLACEMENT_3D('',#18646,#13285,#13286) ;
#10649 = AXIS2_PLACEMENT_3D('',#18648,#13287,#13288) ;
#10650 = AXIS2_PLACEMENT_3D('',#18650,#13290,#13291) ;
#10651 = AXIS2_PLACEMENT_3D('',#18652,#13292,#13293) ;
#10652 = AXIS2_PLACEMENT_3D('',#18653,#13294,#13295) ;
#10653 = AXIS2_PLACEMENT_3D('',#18655,#13296,#13297) ;
#10654 = AXIS2_PLACEMENT_3D('',#18657,#13299,#13300) ;
#10655 = AXIS2_PLACEMENT_3D('',#18659,#13301,#13302) ;
#10656 = AXIS2_PLACEMENT_3D('',#18660,#13303,#13304) ;
#10657 = AXIS2_PLACEMENT_3D('',#18662,#13306,#13307) ;
#10658 = AXIS2_PLACEMENT_3D('',#18663,#13308,#13309) ;
#10659 = AXIS2_PLACEMENT_3D('',#18664,#13310,#13311) ;
#10660 = AXIS2_PLACEMENT_3D('',#18665,#13312,#13313) ;
#10661 = AXIS2_PLACEMENT_3D('',#18666,#13314,#13315) ;
#10662 = AXIS2_PLACEMENT_3D('',#18667,#13316,#13317) ;
#10663 = AXIS2_PLACEMENT_3D('',#18668,#13318,#13319) ;
#10664 = AXIS2_PLACEMENT_3D('',#18669,#13320,#13321) ;
#10665 = AXIS2_PLACEMENT_3D('',#18670,#13322,#13323) ;
#10666 = AXIS2_PLACEMENT_3D('',#18671,#13324,#13325) ;
#10667 = AXIS2_PLACEMENT_3D('',#18672,#13326,#13327) ;
#10668 = AXIS2_PLACEMENT_3D('',#18673,#13328,#13329) ;
#10669 = AXIS2_PLACEMENT_3D('',#18674,#13330,#13331) ;
#10670 = AXIS2_PLACEMENT_3D('',#18675,#13332,#13333) ;
#10671 = AXIS2_PLACEMENT_3D('',#18676,#13334,#13335) ;
#10672 = AXIS2_PLACEMENT_3D('',#18677,#13336,#13337) ;
#10673 = AXIS2_PLACEMENT_3D('',#18678,#13338,#13339) ;
#10674 = AXIS2_PLACEMENT_3D('',#18679,#13340,#13341) ;
#10675 = AXIS2_PLACEMENT_3D('',#18680,#13342,#13343) ;
#10676 = AXIS2_PLACEMENT_3D('',#18681,#13344,#13345) ;
#10677 = AXIS2_PLACEMENT_3D('',#18682,#13346,#13347) ;
#10678 = AXIS2_PLACEMENT_3D('',#18683,#13348,#13349) ;
#10679 = AXIS2_PLACEMENT_3D('',#18684,#13350,#13351) ;
#10680 = AXIS2_PLACEMENT_3D('',#18685,#13352,#13353) ;
#10681 = AXIS2_PLACEMENT_3D('',#18686,#13354,#13355) ;
#10682 = AXIS2_PLACEMENT_3D('',#18687,#13356,#13357) ;
#10683 = AXIS2_PLACEMENT_3D('',#18688,#13358,#13359) ;
#10684 = AXIS2_PLACEMENT_3D('',#18689,#13360,#13361) ;
#10685 = AXIS2_PLACEMENT_3D('',#18690,#13362,#13363) ;
#10686 = AXIS2_PLACEMENT_3D('',#18691,#13364,#13365) ;
#10687 = AXIS2_PLACEMENT_3D('',#18692,#13366,#13367) ;
#10688 = AXIS2_PLACEMENT_3D('',#18693,#13368,#13369) ;
#10689 = AXIS2_PLACEMENT_3D('',#18694,#13370,#13371) ;
#10690 = AXIS2_PLACEMENT_3D('',#18695,#13372,#13373) ;
#10691 = AXIS2_PLACEMENT_3D('',#18696,#13374,#13375) ;
#10692 = AXIS2_PLACEMENT_3D('',#18697,#13376,#13377) ;
#10693 = AXIS2_PLACEMENT_3D('',#18698,#13378,#13379) ;
#10694 = AXIS2_PLACEMENT_3D('',#18699,#13380,#13381) ;
#10695 = AXIS2_PLACEMENT_3D('',#18700,#13382,#13383) ;
#10696 = AXIS2_PLACEMENT_3D('',#18701,#13384,#13385) ;
#10697 = AXIS2_PLACEMENT_3D('',#18702,#13386,#13387) ;
#10698 = AXIS2_PLACEMENT_3D('',#18703,#13388,#13389) ;
#10699 = AXIS2_PLACEMENT_3D('',#18704,#13390,#13391) ;
#10700 = AXIS2_PLACEMENT_3D('',#18705,#13392,#13393) ;
#10701 = AXIS2_PLACEMENT_3D('',#18706,#13394,#13395) ;
#10702 = AXIS2_PLACEMENT_3D('',#18707,#13396,#13397) ;
#10703 = AXIS2_PLACEMENT_3D('',#18708,#13398,#13399) ;
#10704 = AXIS2_PLACEMENT_3D('',#18709,#13400,#13401) ;
#10705 = AXIS2_PLACEMENT_3D('',#18710,#13402,#13403) ;
#10706 = AXIS2_PLACEMENT_3D('',#18711,#13404,#13405) ;
#10707 = AXIS2_PLACEMENT_3D('',#18712,#13406,#13407) ;
#10708 = AXIS2_PLACEMENT_3D('',#18713,#13408,#13409) ;
#10709 = AXIS2_PLACEMENT_3D('',#18714,#13410,#13411) ;
#10710 = AXIS2_PLACEMENT_3D('',#18715,#13412,#13413) ;
#10711 = AXIS2_PLACEMENT_3D('',#18716,#13414,#13415) ;
#10712 = AXIS2_PLACEMENT_3D('',#18717,#13416,#13417) ;
#10713 = AXIS2_PLACEMENT_3D('',#18718,#13418,#13419) ;
#10714 = AXIS2_PLACEMENT_3D('',#18719,#13420,#13421) ;
#10715 = DIRECTION('axis',(0.,0.,1.)) ;
#10716 = DIRECTION('refdir',(1.,0.,0.)) ;
#10717 = DIRECTION('axis',(0.,0.,1.)) ;
#10718 = DIRECTION('refdir',(1.,0.,0.)) ;
#10719 = DIRECTION('center_axis',(0.,0.,-1.)) ;
#10720 = DIRECTION('ref_axis',(1.,0.,0.)) ;
#10721 = DIRECTION('center_axis',(0.,0.,-1.)) ;
#10722 = DIRECTION('ref_axis',(1.,0.,0.)) ;
#10723 = DIRECTION('',(0.707106781186558,-8.65956056235506E-17,0.707106781186537)) ;
#10724 = DIRECTION('center_axis',(0.,0.,1.)) ;
#10725 = DIRECTION('ref_axis',(1.,0.,0.)) ;
#10726 = DIRECTION('center_axis',(0.,0.,1.)) ;
#10727 = DIRECTION('ref_axis',(1.,0.,0.)) ;
#10728 = DIRECTION('',(0.,-1.,0.)) ;
#10729 = DIRECTION('',(-1.,0.,0.)) ;
#10730 = DIRECTION('',(0.,1.,0.)) ;
#10731 = DIRECTION('',(1.,0.,0.)) ;
#10732 = DIRECTION('center_axis',(0.,0.,-1.)) ;
#10733 = DIRECTION('ref_axis',(1.,0.,0.)) ;
#10734 = DIRECTION('center_axis',(0.,0.,1.)) ;
#10735 = DIRECTION('ref_axis',(1.,0.,0.)) ;
#10736 = DIRECTION('',(0.,0.,1.)) ;
#10737 = DIRECTION('center_axis',(0.,0.,1.)) ;
#10738 = DIRECTION('ref_axis',(1.,0.,0.)) ;
#10739 = DIRECTION('center_axis',(0.,0.,-1.)) ;
#10740 = DIRECTION('ref_axis',(1.,0.,0.)) ;
#10741 = DIRECTION('center_axis',(0.,0.,-1.)) ;
#10742 = DIRECTION('ref_axis',(1.,0.,0.)) ;
#10743 = DIRECTION('',(0.707106781186558,-8.65956056235506E-17,0.707106781186537)) ;
#10744 = DIRECTION('center_axis',(0.,0.,1.)) ;
#10745 = DIRECTION('ref_axis',(1.,0.,0.)) ;
#10746 = DIRECTION('center_axis',(0.,0.,1.)) ;
#10747 = DIRECTION('ref_axis',(1.,0.,0.)) ;
#10748 = DIRECTION('',(0.,-1.,0.)) ;
#10749 = DIRECTION('',(-1.,0.,0.)) ;
#10750 = DIRECTION('',(0.,1.,0.)) ;
#10751 = DIRECTION('',(1.,0.,0.)) ;
#10752 = DIRECTION('center_axis',(0.,0.,-1.)) ;
#10753 = DIRECTION('ref_axis',(1.,0.,0.)) ;
#10754 = DIRECTION('center_axis',(0.,0.,1.)) ;
#10755 = DIRECTION('ref_axis',(1.,0.,0.)) ;
#10756 = DIRECTION('',(0.,0.,1.)) ;
#10757 = DIRECTION('center_axis',(0.,0.,1.)) ;
#10758 = DIRECTION('ref_axis',(1.,0.,0.)) ;
#10759 = DIRECTION('center_axis',(0.,0.,-1.)) ;
#10760 = DIRECTION('ref_axis',(1.,0.,0.)) ;
#10761 = DIRECTION('center_axis',(0.,0.,-1.)) ;
#10762 = DIRECTION('ref_axis',(1.,0.,0.)) ;
#10763 = DIRECTION('',(0.707106781186558,-8.65956056235506E-17,0.707106781186537)) ;
#10764 = DIRECTION('center_axis',(0.,0.,1.)) ;
#10765 = DIRECTION('ref_axis',(1.,0.,0.)) ;
#10766 = DIRECTION('center_axis',(0.,0.,1.)) ;
#10767 = DIRECTION('ref_axis',(1.,0.,0.)) ;
#10768 = DIRECTION('',(0.,-1.,0.)) ;
#10769 = DIRECTION('',(-1.,0.,0.)) ;
#10770 = DIRECTION('',(0.,1.,0.)) ;
#10771 = DIRECTION('',(1.,0.,0.)) ;
#10772 = DIRECTION('center_axis',(0.,0.,-1.)) ;
#10773 = DIRECTION('ref_axis',(1.,0.,0.)) ;
#10774 = DIRECTION('center_axis',(0.,0.,1.)) ;
#10775 = DIRECTION('ref_axis',(1.,0.,0.)) ;
#10776 = DIRECTION('',(0.,0.,1.)) ;
#10777 = DIRECTION('center_axis',(0.,0.,1.)) ;
#10778 = DIRECTION('ref_axis',(1.,0.,0.)) ;
#10779 = DIRECTION('center_axis',(0.,0.,-1.)) ;
#10780 = DIRECTION('ref_axis',(1.,0.,0.)) ;
#10781 = DIRECTION('center_axis',(0.,0.,-1.)) ;
#10782 = DIRECTION('ref_axis',(1.,0.,0.)) ;
#10783 = DIRECTION('',(0.707106781186558,-8.65956056235506E-17,0.707106781186537)) ;
#10784 = DIRECTION('center_axis',(0.,0.,1.)) ;
#10785 = DIRECTION('ref_axis',(1.,0.,0.)) ;
#10786 = DIRECTION('center_axis',(0.,0.,1.)) ;
#10787 = DIRECTION('ref_axis',(1.,0.,0.)) ;
#10788 = DIRECTION('',(0.,-1.,0.)) ;
#10789 = DIRECTION('',(-1.,0.,0.)) ;
#10790 = DIRECTION('',(0.,1.,0.)) ;
#10791 = DIRECTION('',(1.,0.,0.)) ;
#10792 = DIRECTION('center_axis',(0.,0.,-1.)) ;
#10793 = DIRECTION('ref_axis',(1.,0.,0.)) ;
#10794 = DIRECTION('center_axis',(0.,0.,1.)) ;
#10795 = DIRECTION('ref_axis',(1.,0.,0.)) ;
#10796 = DIRECTION('',(0.,0.,1.)) ;
#10797 = DIRECTION('center_axis',(0.,0.,1.)) ;
#10798 = DIRECTION('ref_axis',(1.,0.,0.)) ;
#10799 = DIRECTION('center_axis',(0.,0.,-1.)) ;
#10800 = DIRECTION('ref_axis',(1.,0.,0.)) ;
#10801 = DIRECTION('',(0.707106781186537,-8.6595605623548E-17,0.707106781186558)) ;
#10802 = DIRECTION('center_axis',(0.,0.,1.)) ;
#10803 = DIRECTION('ref_axis',(1.,0.,0.)) ;
#10804 = DIRECTION('center_axis',(0.,0.,1.)) ;
#10805 = DIRECTION('ref_axis',(1.,0.,0.)) ;
#10806 = DIRECTION('',(0.,0.,1.)) ;
#10807 = DIRECTION('center_axis',(0.,0.,1.)) ;
#10808 = DIRECTION('ref_axis',(1.,0.,0.)) ;
#10809 = DIRECTION('center_axis',(0.,0.,1.)) ;
#10810 = DIRECTION('ref_axis',(1.,0.,0.)) ;
#10811 = DIRECTION('center_axis',(0.,0.,-1.)) ;
#10812 = DIRECTION('ref_axis',(1.,0.,0.)) ;
#10813 = DIRECTION('',(0.707106781186537,-8.6595605623548E-17,0.707106781186558)) ;
#10814 = DIRECTION('center_axis',(0.,0.,1.)) ;
#10815 = DIRECTION('ref_axis',(1.,0.,0.)) ;
#10816 = DIRECTION('center_axis',(0.,0.,1.)) ;
#10817 = DIRECTION('ref_axis',(1.,0.,0.)) ;
#10818 = DIRECTION('',(0.,0.,1.)) ;
#10819 = DIRECTION('center_axis',(0.,0.,1.)) ;
#10820 = DIRECTION('ref_axis',(1.,0.,0.)) ;
#10821 = DIRECTION('center_axis',(0.,0.,1.)) ;
#10822 = DIRECTION('ref_axis',(1.,0.,0.)) ;
#10823 = DIRECTION('center_axis',(0.,0.,-1.)) ;
#10824 = DIRECTION('ref_axis',(1.,0.,0.)) ;
#10825 = DIRECTION('',(0.707106781186537,-8.6595605623548E-17,0.707106781186558)) ;
#10826 = DIRECTION('center_axis',(0.,0.,1.)) ;
#10827 = DIRECTION('ref_axis',(1.,0.,0.)) ;
#10828 = DIRECTION('center_axis',(0.,0.,1.)) ;
#10829 = DIRECTION('ref_axis',(1.,0.,0.)) ;
#10830 = DIRECTION('',(0.,0.,1.)) ;
#10831 = DIRECTION('center_axis',(0.,0.,1.)) ;
#10832 = DIRECTION('ref_axis',(1.,0.,0.)) ;
#10833 = DIRECTION('center_axis',(0.,0.,-1.)) ;
#10834 = DIRECTION('ref_axis',(1.,0.,0.)) ;
#10835 = DIRECTION('',(0.707106781186537,-8.6595605623548E-17,0.707106781186558)) ;
#10836 = DIRECTION('center_axis',(0.,0.,1.)) ;
#10837 = DIRECTION('ref_axis',(1.,0.,0.)) ;
#10838 = DIRECTION('center_axis',(0.,0.,1.)) ;
#10839 = DIRECTION('ref_axis',(1.,0.,0.)) ;
#10840 = DIRECTION('',(0.,0.,1.)) ;
#10841 = DIRECTION('center_axis',(0.,0.,1.)) ;
#10842 = DIRECTION('ref_axis',(1.,0.,0.)) ;
#10843 = DIRECTION('center_axis',(0.,0.,-1.)) ;
#10844 = DIRECTION('ref_axis',(1.,0.,0.)) ;
#10845 = DIRECTION('',(0.857167300702109,1.04972719113861E-16,0.51503807491006)) ;
#10846 = DIRECTION('center_axis',(0.,0.,-1.)) ;
#10847 = DIRECTION('ref_axis',(1.,0.,0.)) ;
#10848 = DIRECTION('',(0.857167300702111,1.04972719113862E-16,0.515038074910057)) ;
#10849 = DIRECTION('center_axis',(0.,0.,-1.)) ;
#10850 = DIRECTION('ref_axis',(1.,0.,0.)) ;
#10851 = DIRECTION('',(0.857167300702109,1.04972719113861E-16,0.51503807491006)) ;
#10852 = DIRECTION('center_axis',(0.,0.,-1.)) ;
#10853 = DIRECTION('ref_axis',(1.,0.,0.)) ;
#10854 = DIRECTION('',(0.857167300702111,1.04972719113862E-16,0.515038074910057)) ;
#10855 = DIRECTION('center_axis',(0.,0.,-1.)) ;
#10856 = DIRECTION('ref_axis',(-1.,1.25569625557165E-14,0.)) ;
#10857 = DIRECTION('center_axis',(0.,1.,0.)) ;
#10858 = DIRECTION('ref_axis',(1.,0.,0.)) ;
#10859 = DIRECTION('center_axis',(0.,1.,0.)) ;
#10860 = DIRECTION('ref_axis',(1.,0.,0.)) ;
#10861 = DIRECTION('',(0.,1.,0.)) ;
#10862 = DIRECTION('center_axis',(0.,-1.,0.)) ;
#10863 = DIRECTION('ref_axis',(1.,0.,0.)) ;
#10864 = DIRECTION('center_axis',(0.,0.,-1.)) ;
#10865 = DIRECTION('ref_axis',(1.,0.,0.)) ;
#10866 = DIRECTION('',(0.857167300702113,1.04972719113862E-16,0.515038074910054)) ;
#10867 = DIRECTION('center_axis',(0.,0.,-1.)) ;
#10868 = DIRECTION('ref_axis',(-1.,-1.2312033195887E-14,0.)) ;
#10869 = DIRECTION('center_axis',(0.,1.,0.)) ;
#10870 = DIRECTION('ref_axis',(1.,0.,0.)) ;
#10871 = DIRECTION('center_axis',(0.,1.,0.)) ;
#10872 = DIRECTION('ref_axis',(1.,0.,0.)) ;
#10873 = DIRECTION('',(0.,1.,0.)) ;
#10874 = DIRECTION('center_axis',(0.,-1.,0.)) ;
#10875 = DIRECTION('ref_axis',(1.,0.,0.)) ;
#10876 = DIRECTION('center_axis',(0.,0.,-1.)) ;
#10877 = DIRECTION('ref_axis',(1.,0.,0.)) ;
#10878 = DIRECTION('',(0.857167300702113,1.04972719113862E-16,0.515038074910054)) ;
#10879 = DIRECTION('center_axis',(-1.,0.,0.)) ;
#10880 = DIRECTION('ref_axis',(0.,0.,-1.)) ;
#10881 = DIRECTION('',(-1.,0.,0.)) ;
#10882 = DIRECTION('center_axis',(0.,0.,-1.)) ;
#10883 = DIRECTION('ref_axis',(1.,0.,0.)) ;
#10884 = DIRECTION('center_axis',(0.,0.,-1.)) ;
#10885 = DIRECTION('ref_axis',(1.,0.,0.)) ;
#10886 = DIRECTION('',(0.,0.,-1.)) ;
#10887 = DIRECTION('center_axis',(0.,0.,-1.)) ;
#10888 = DIRECTION('ref_axis',(1.,0.,0.)) ;
#10889 = DIRECTION('center_axis',(0.,0.,1.)) ;
#10890 = DIRECTION('ref_axis',(1.,0.,0.)) ;
#10891 = DIRECTION('center_axis',(-1.,0.,0.)) ;
#10892 = DIRECTION('ref_axis',(0.,0.,-1.)) ;
#10893 = DIRECTION('',(-1.,0.,0.)) ;
#10894 = DIRECTION('center_axis',(0.,0.,-1.)) ;
#10895 = DIRECTION('ref_axis',(1.,0.,0.)) ;
#10896 = DIRECTION('center_axis',(0.,0.,-1.)) ;
#10897 = DIRECTION('ref_axis',(1.,0.,0.)) ;
#10898 = DIRECTION('',(0.,0.,-1.)) ;
#10899 = DIRECTION('center_axis',(0.,0.,-1.)) ;
#10900 = DIRECTION('ref_axis',(1.,0.,0.)) ;
#10901 = DIRECTION('center_axis',(0.,0.,1.)) ;
#10902 = DIRECTION('ref_axis',(1.,0.,0.)) ;
#10903 = DIRECTION('center_axis',(0.,1.,0.)) ;
#10904 = DIRECTION('ref_axis',(1.,0.,0.)) ;
#10905 = DIRECTION('center_axis',(0.,1.,0.)) ;
#10906 = DIRECTION('ref_axis',(1.,0.,0.)) ;
#10907 = DIRECTION('',(0.,1.,0.)) ;
#10908 = DIRECTION('center_axis',(0.,-1.,0.)) ;
#10909 = DIRECTION('ref_axis',(1.,0.,0.)) ;
#10910 = DIRECTION('center_axis',(0.,1.,0.)) ;
#10911 = DIRECTION('ref_axis',(1.,0.,0.)) ;
#10912 = DIRECTION('center_axis',(0.,1.,0.)) ;
#10913 = DIRECTION('ref_axis',(1.,0.,0.)) ;
#10914 = DIRECTION('',(0.,1.,0.)) ;
#10915 = DIRECTION('center_axis',(0.,-1.,0.)) ;
#10916 = DIRECTION('ref_axis',(1.,0.,0.)) ;
#10917 = DIRECTION('center_axis',(0.,1.,0.)) ;
#10918 = DIRECTION('ref_axis',(1.,0.,0.)) ;
#10919 = DIRECTION('',(0.,-1.,0.)) ;
#10920 = DIRECTION('center_axis',(0.,-1.,0.)) ;
#10921 = DIRECTION('ref_axis',(1.,0.,0.)) ;
#10922 = DIRECTION('',(0.,1.,0.)) ;
#10923 = DIRECTION('center_axis',(0.,1.,0.)) ;
#10924 = DIRECTION('ref_axis',(1.,0.,0.)) ;
#10925 = DIRECTION('center_axis',(0.,1.,0.)) ;
#10926 = DIRECTION('ref_axis',(1.,0.,0.)) ;
#10927 = DIRECTION('',(0.,-1.,0.)) ;
#10928 = DIRECTION('center_axis',(0.,-1.,0.)) ;
#10929 = DIRECTION('ref_axis',(1.,0.,0.)) ;
#10930 = DIRECTION('',(0.,1.,0.)) ;
#10931 = DIRECTION('center_axis',(0.,1.,0.)) ;
#10932 = DIRECTION('ref_axis',(1.,0.,0.)) ;
#10933 = DIRECTION('center_axis',(-1.,0.,0.)) ;
#10934 = DIRECTION('ref_axis',(0.,0.,1.)) ;
#10935 = DIRECTION('',(0.,0.,1.)) ;
#10936 = DIRECTION('',(0.,1.,0.)) ;
#10937 = DIRECTION('',(0.,0.,1.)) ;
#10938 = DIRECTION('center_axis',(0.,1.,0.)) ;
#10939 = DIRECTION('ref_axis',(1.,0.,0.)) ;
#10940 = DIRECTION('center_axis',(0.,1.,0.)) ;
#10941 = DIRECTION('ref_axis',(-1.,0.,0.)) ;
#10942 = DIRECTION('',(1.,0.,0.)) ;
#10943 = DIRECTION('',(0.,0.,1.)) ;
#10944 = DIRECTION('',(-1.,0.,0.)) ;
#10945 = DIRECTION('center_axis',(-1.,0.,0.)) ;
#10946 = DIRECTION('ref_axis',(0.,0.,1.)) ;
#10947 = DIRECTION('',(0.,0.,1.)) ;
#10948 = DIRECTION('',(0.,1.,0.)) ;
#10949 = DIRECTION('',(0.,0.,1.)) ;
#10950 = DIRECTION('center_axis',(0.,1.,0.)) ;
#10951 = DIRECTION('ref_axis',(1.,0.,0.)) ;
#10952 = DIRECTION('center_axis',(0.,1.,0.)) ;
#10953 = DIRECTION('ref_axis',(-1.,0.,0.)) ;
#10954 = DIRECTION('',(1.,0.,0.)) ;
#10955 = DIRECTION('',(0.,0.,1.)) ;
#10956 = DIRECTION('',(-1.,0.,0.)) ;
#10957 = DIRECTION('center_axis',(0.,0.707106781186548,0.707106781186548)) ;
#10958 = DIRECTION('ref_axis',(1.,0.,0.)) ;
#10959 = DIRECTION('',(0.,-0.707106781186548,0.707106781186548)) ;
#10960 = DIRECTION('',(1.,0.,0.)) ;
#10961 = DIRECTION('',(0.,0.707106781186548,-0.707106781186548)) ;
#10962 = DIRECTION('',(-1.,0.,0.)) ;
#10963 = DIRECTION('center_axis',(0.,1.,0.)) ;
#10964 = DIRECTION('ref_axis',(-1.,0.,0.)) ;
#10965 = DIRECTION('',(0.,0.,1.)) ;
#10966 = DIRECTION('',(-1.,0.,0.)) ;
#10967 = DIRECTION('',(-1.,0.,0.)) ;
#10968 = DIRECTION('',(-1.,0.,0.)) ;
#10969 = DIRECTION('',(0.,0.,1.)) ;
#10970 = DIRECTION('center_axis',(1.,0.,0.)) ;
#10971 = DIRECTION('ref_axis',(0.,1.,0.)) ;
#10972 = DIRECTION('',(0.,1.,0.)) ;
#10973 = DIRECTION('',(0.,0.,-1.)) ;
#10974 = DIRECTION('',(0.,-1.,0.)) ;
#10975 = DIRECTION('',(0.,0.,1.)) ;
#10976 = DIRECTION('',(0.,1.,0.)) ;
#10977 = DIRECTION('',(0.,0.,-1.)) ;
#10978 = DIRECTION('',(0.,-1.,0.)) ;
#10979 = DIRECTION('',(0.,0.,1.)) ;
#10980 = DIRECTION('',(0.,1.,0.)) ;
#10981 = DIRECTION('',(0.,0.707106781186548,0.707106781186548)) ;
#10982 = DIRECTION('',(0.,0.,1.)) ;
#10983 = DIRECTION('',(0.,1.,0.)) ;
#10984 = DIRECTION('',(0.,0.,1.)) ;
#10985 = DIRECTION('',(0.,0.,1.)) ;
#10986 = DIRECTION('',(0.,1.,0.)) ;
#10987 = DIRECTION('',(0.,0.,1.)) ;
#10988 = DIRECTION('',(0.,0.,1.)) ;
#10989 = DIRECTION('',(0.,1.,0.)) ;
#10990 = DIRECTION('center_axis',(0.,-0.707106781186548,0.707106781186548)) ;
#10991 = DIRECTION('ref_axis',(1.,0.,0.)) ;
#10992 = DIRECTION('',(-1.,0.,0.)) ;
#10993 = DIRECTION('',(0.,-0.707106781186548,-0.707106781186548)) ;
#10994 = DIRECTION('',(1.,0.,0.)) ;
#10995 = DIRECTION('center_axis',(0.,-1.,0.)) ;
#10996 = DIRECTION('ref_axis',(1.,0.,0.)) ;
#10997 = DIRECTION('',(0.,0.,1.)) ;
#10998 = DIRECTION('',(1.,0.,0.)) ;
#10999 = DIRECTION('',(1.,0.,0.)) ;
#11000 = DIRECTION('',(1.,0.,0.)) ;
#11001 = DIRECTION('center_axis',(0.,0.,1.)) ;
#11002 = DIRECTION('ref_axis',(1.,0.,0.)) ;
#11003 = DIRECTION('center_axis',(0.,0.,1.)) ;
#11004 = DIRECTION('ref_axis',(1.,0.,0.)) ;
#11005 = DIRECTION('',(0.,0.,-1.)) ;
#11006 = DIRECTION('center_axis',(0.,0.,1.)) ;
#11007 = DIRECTION('ref_axis',(1.,0.,0.)) ;
#11008 = DIRECTION('',(0.,0.,-1.)) ;
#11009 = DIRECTION('center_axis',(0.,0.,-1.)) ;
#11010 = DIRECTION('ref_axis',(1.,0.,0.)) ;
#11011 = DIRECTION('center_axis',(0.,0.,1.)) ;
#11012 = DIRECTION('ref_axis',(1.,0.,0.)) ;
#11013 = DIRECTION('center_axis',(0.,0.,-1.)) ;
#11014 = DIRECTION('ref_axis',(1.,0.,0.)) ;
#11015 = DIRECTION('',(0.,0.,1.)) ;
#11016 = DIRECTION('center_axis',(0.,0.,1.)) ;
#11017 = DIRECTION('ref_axis',(1.,0.,0.)) ;
#11018 = DIRECTION('center_axis',(0.,0.,-1.)) ;
#11019 = DIRECTION('ref_axis',(-1.,0.,0.)) ;
#11020 = DIRECTION('center_axis',(0.,0.,-1.)) ;
#11021 = DIRECTION('ref_axis',(-1.,0.,0.)) ;
#11022 = DIRECTION('',(0.,1.,0.)) ;
#11023 = DIRECTION('center_axis',(0.,0.,1.)) ;
#11024 = DIRECTION('ref_axis',(1.,0.,0.)) ;
#11025 = DIRECTION('center_axis',(-1.,0.,0.)) ;
#11026 = DIRECTION('ref_axis',(0.,-1.,0.)) ;
#11027 = DIRECTION('',(0.,-1.,0.)) ;
#11028 = DIRECTION('',(0.,0.,-1.)) ;
#11029 = DIRECTION('',(0.,1.,0.)) ;
#11030 = DIRECTION('',(0.,0.,1.)) ;
#11031 = DIRECTION('',(0.,-1.,0.)) ;
#11032 = DIRECTION('',(0.,0.,1.)) ;
#11033 = DIRECTION('',(0.,-1.,0.)) ;
#11034 = DIRECTION('',(0.,-1.,0.)) ;
#11035 = DIRECTION('',(0.,-1.,0.)) ;
#11036 = DIRECTION('',(0.,0.,-1.)) ;
#11037 = DIRECTION('',(0.,-1.,0.)) ;
#11038 = DIRECTION('',(0.,-1.,0.)) ;
#11039 = DIRECTION('',(0.,0.,-1.)) ;
#11040 = DIRECTION('',(0.,1.,0.)) ;
#11041 = DIRECTION('',(0.,-1.,0.)) ;
#11042 = DIRECTION('',(0.,0.,-1.)) ;
#11043 = DIRECTION('',(0.,1.,0.)) ;
#11044 = DIRECTION('center_axis',(0.,0.,1.)) ;
#11045 = DIRECTION('ref_axis',(1.,0.,0.)) ;
#11046 = DIRECTION('center_axis',(0.,0.,-1.)) ;
#11047 = DIRECTION('ref_axis',(1.,0.,0.)) ;
#11048 = DIRECTION('center_axis',(0.,0.,-1.)) ;
#11049 = DIRECTION('ref_axis',(-1.,0.,0.)) ;
#11050 = DIRECTION('',(-1.,0.,0.)) ;
#11051 = DIRECTION('center_axis',(0.,0.,1.)) ;
#11052 = DIRECTION('ref_axis',(1.,0.,0.)) ;
#11053 = DIRECTION('',(1.,0.,0.)) ;
#11054 = DIRECTION('',(0.,1.,0.)) ;
#11055 = DIRECTION('center_axis',(0.,1.,0.)) ;
#11056 = DIRECTION('ref_axis',(-1.,0.,0.)) ;
#11057 = DIRECTION('center_axis',(0.,1.,0.)) ;
#11058 = DIRECTION('ref_axis',(-1.,0.,0.)) ;
#11059 = DIRECTION('center_axis',(0.,1.,0.)) ;
#11060 = DIRECTION('ref_axis',(1.,0.,0.)) ;
#11061 = DIRECTION('center_axis',(0.,0.,1.)) ;
#11062 = DIRECTION('ref_axis',(1.,0.,0.)) ;
#11063 = DIRECTION('',(0.,1.,0.)) ;
#11064 = DIRECTION('',(-1.,0.,0.)) ;
#11065 = DIRECTION('',(0.,1.,0.)) ;
#11066 = DIRECTION('',(-1.,0.,0.)) ;
#11067 = DIRECTION('center_axis',(0.,1.,0.)) ;
#11068 = DIRECTION('ref_axis',(-1.,0.,0.)) ;
#11069 = DIRECTION('',(0.,0.,-1.)) ;
#11070 = DIRECTION('',(0.,0.,1.)) ;
#11071 = DIRECTION('',(-1.,0.,0.)) ;
#11072 = DIRECTION('center_axis',(1.,0.,0.)) ;
#11073 = DIRECTION('ref_axis',(0.,1.,0.)) ;
#11074 = DIRECTION('',(0.,1.,0.)) ;
#11075 = DIRECTION('',(0.,0.,1.)) ;
#11076 = DIRECTION('center_axis',(0.,0.,1.)) ;
#11077 = DIRECTION('ref_axis',(1.,0.,0.)) ;
#11078 = DIRECTION('center_axis',(0.,0.,1.)) ;
#11079 = DIRECTION('ref_axis',(1.,0.,0.)) ;
#11080 = DIRECTION('',(0.,0.,-1.)) ;
#11081 = DIRECTION('center_axis',(0.,0.,1.)) ;
#11082 = DIRECTION('ref_axis',(1.,0.,0.)) ;
#11083 = DIRECTION('center_axis',(0.,0.,1.)) ;
#11084 = DIRECTION('ref_axis',(1.,0.,0.)) ;
#11085 = DIRECTION('center_axis',(0.,0.,-1.)) ;
#11086 = DIRECTION('ref_axis',(1.,0.,0.)) ;
#11087 = DIRECTION('center_axis',(0.,0.,1.)) ;
#11088 = DIRECTION('ref_axis',(1.,0.,0.)) ;
#11089 = DIRECTION('center_axis',(0.,0.,-1.)) ;
#11090 = DIRECTION('ref_axis',(-1.,0.,0.)) ;
#11091 = DIRECTION('center_axis',(0.,0.,-1.)) ;
#11092 = DIRECTION('ref_axis',(-1.,0.,0.)) ;
#11093 = DIRECTION('center_axis',(0.,0.,1.)) ;
#11094 = DIRECTION('ref_axis',(1.,0.,0.)) ;
#11095 = DIRECTION('center_axis',(0.,0.,-1.)) ;
#11096 = DIRECTION('ref_axis',(-1.,0.,0.)) ;
#11097 = DIRECTION('',(-1.,0.,0.)) ;
#11098 = DIRECTION('center_axis',(0.,0.,1.)) ;
#11099 = DIRECTION('ref_axis',(1.,0.,0.)) ;
#11100 = DIRECTION('',(1.,0.,0.)) ;
#11101 = DIRECTION('',(0.,1.,0.)) ;
#11102 = DIRECTION('center_axis',(0.,1.,0.)) ;
#11103 = DIRECTION('ref_axis',(-1.,0.,0.)) ;
#11104 = DIRECTION('center_axis',(0.,1.,0.)) ;
#11105 = DIRECTION('ref_axis',(-1.,0.,0.)) ;
#11106 = DIRECTION('center_axis',(0.,1.,0.)) ;
#11107 = DIRECTION('ref_axis',(1.,0.,0.)) ;
#11108 = DIRECTION('center_axis',(0.,0.,1.)) ;
#11109 = DIRECTION('ref_axis',(1.,0.,0.)) ;
#11110 = DIRECTION('',(0.,1.,0.)) ;
#11111 = DIRECTION('',(1.,0.,0.)) ;
#11112 = DIRECTION('',(0.,1.,0.)) ;
#11113 = DIRECTION('',(1.,0.,0.)) ;
#11114 = DIRECTION('center_axis',(0.,-1.,0.)) ;
#11115 = DIRECTION('ref_axis',(1.,0.,0.)) ;
#11116 = DIRECTION('',(0.,0.,1.)) ;
#11117 = DIRECTION('',(1.,0.,0.)) ;
#11118 = DIRECTION('',(0.,0.,1.)) ;
#11119 = DIRECTION('center_axis',(1.,0.,0.)) ;
#11120 = DIRECTION('ref_axis',(0.,1.,0.)) ;
#11121 = DIRECTION('',(0.,1.,0.)) ;
#11122 = DIRECTION('',(0.,0.,-1.)) ;
#11123 = DIRECTION('center_axis',(0.,0.,1.)) ;
#11124 = DIRECTION('ref_axis',(1.,0.,0.)) ;
#11125 = DIRECTION('',(0.,-1.,0.)) ;
#11126 = DIRECTION('',(1.,0.,0.)) ;
#11127 = DIRECTION('',(0.,1.,0.)) ;
#11128 = DIRECTION('center_axis',(0.,1.,0.)) ;
#11129 = DIRECTION('ref_axis',(-1.,0.,0.)) ;
#11130 = DIRECTION('',(0.,0.,1.)) ;
#11131 = DIRECTION('',(-1.,0.,0.)) ;
#11132 = DIRECTION('',(0.,0.,1.)) ;
#11133 = DIRECTION('center_axis',(1.,0.,0.)) ;
#11134 = DIRECTION('ref_axis',(0.,1.,0.)) ;
#11135 = DIRECTION('',(0.,1.,0.)) ;
#11136 = DIRECTION('',(0.,0.,1.)) ;
#11137 = DIRECTION('center_axis',(0.,-1.,0.)) ;
#11138 = DIRECTION('ref_axis',(1.,0.,0.)) ;
#11139 = DIRECTION('',(0.,0.,1.)) ;
#11140 = DIRECTION('center_axis',(0.,0.,1.)) ;
#11141 = DIRECTION('ref_axis',(1.,0.,0.)) ;
#11142 = DIRECTION('',(0.,1.,0.)) ;
#11143 = DIRECTION('',(-1.,0.,0.)) ;
#11144 = DIRECTION('',(0.,-1.,0.)) ;
#11145 = DIRECTION('center_axis',(0.,1.,0.)) ;
#11146 = DIRECTION('ref_axis',(-1.,0.,0.)) ;
#11147 = DIRECTION('',(0.,0.,1.)) ;
#11148 = DIRECTION('',(0.,0.,1.)) ;
#11149 = DIRECTION('center_axis',(1.,0.,0.)) ;
#11150 = DIRECTION('ref_axis',(0.,1.,0.)) ;
#11151 = DIRECTION('',(0.,1.,0.)) ;
#11152 = DIRECTION('',(0.,0.,1.)) ;
#11153 = DIRECTION('center_axis',(0.,-1.,0.)) ;
#11154 = DIRECTION('ref_axis',(1.,0.,0.)) ;
#11155 = DIRECTION('',(1.,0.,0.)) ;
#11156 = DIRECTION('',(0.,0.,1.)) ;
#11157 = DIRECTION('center_axis',(0.,0.,1.)) ;
#11158 = DIRECTION('ref_axis',(1.,0.,0.)) ;
#11159 = DIRECTION('',(0.,-1.,0.)) ;
#11160 = DIRECTION('',(0.,-1.,0.)) ;
#11161 = DIRECTION('',(1.,0.,0.)) ;
#11162 = DIRECTION('',(0.,1.,0.)) ;
#11163 = DIRECTION('',(-1.,0.,0.)) ;
#11164 = DIRECTION('',(0.,-1.,0.)) ;
#11165 = DIRECTION('center_axis',(1.,0.,0.)) ;
#11166 = DIRECTION('ref_axis',(0.,1.,0.)) ;
#11167 = DIRECTION('',(0.,0.,-1.)) ;
#11168 = DIRECTION('',(0.,1.,0.)) ;
#11169 = DIRECTION('',(0.,0.,1.)) ;
#11170 = DIRECTION('center_axis',(0.,-1.,0.)) ;
#11171 = DIRECTION('ref_axis',(1.,0.,0.)) ;
#11172 = DIRECTION('',(1.,0.,0.)) ;
#11173 = DIRECTION('',(1.,0.,0.)) ;
#11174 = DIRECTION('center_axis',(0.,0.,1.)) ;
#11175 = DIRECTION('ref_axis',(1.,0.,0.)) ;
#11176 = DIRECTION('',(0.,-1.,0.)) ;
#11177 = DIRECTION('',(1.,0.,0.)) ;
#11178 = DIRECTION('center_axis',(0.,1.,0.)) ;
#11179 = DIRECTION('ref_axis',(-1.,0.,0.)) ;
#11180 = DIRECTION('',(0.,0.,1.)) ;
#11181 = DIRECTION('',(-1.,0.,0.)) ;
#11182 = DIRECTION('',(-1.,0.,0.)) ;
#11183 = DIRECTION('center_axis',(0.,-1.,0.)) ;
#11184 = DIRECTION('ref_axis',(1.,0.,0.)) ;
#11185 = DIRECTION('',(0.,0.,1.)) ;
#11186 = DIRECTION('center_axis',(-1.,0.,0.)) ;
#11187 = DIRECTION('ref_axis',(0.,-1.,0.)) ;
#11188 = DIRECTION('',(0.,-1.,0.)) ;
#11189 = DIRECTION('center_axis',(0.,0.,1.)) ;
#11190 = DIRECTION('ref_axis',(1.,0.,0.)) ;
#11191 = DIRECTION('',(-1.,0.,0.)) ;
#11192 = DIRECTION('center_axis',(0.,0.,1.)) ;
#11193 = DIRECTION('ref_axis',(1.,0.,0.)) ;
#11194 = DIRECTION('',(1.,0.,0.)) ;
#11195 = DIRECTION('center_axis',(0.,0.,1.)) ;
#11196 = DIRECTION('ref_axis',(1.,0.,0.)) ;
#11197 = DIRECTION('',(-1.,0.,0.)) ;
#11198 = DIRECTION('',(0.,-1.,0.)) ;
#11199 = DIRECTION('center_axis',(0.,0.,1.)) ;
#11200 = DIRECTION('ref_axis',(1.,0.,0.)) ;
#11201 = DIRECTION('',(0.,-1.,0.)) ;
#11202 = DIRECTION('',(1.,0.,0.)) ;
#11203 = DIRECTION('center_axis',(0.,1.,0.)) ;
#11204 = DIRECTION('ref_axis',(-1.,0.,0.)) ;
#11205 = DIRECTION('',(0.,0.,1.)) ;
#11206 = DIRECTION('center_axis',(0.,-1.,0.)) ;
#11207 = DIRECTION('ref_axis',(1.,0.,0.)) ;
#11208 = DIRECTION('',(0.,0.,1.)) ;
#11209 = DIRECTION('center_axis',(-1.,0.,0.)) ;
#11210 = DIRECTION('ref_axis',(0.,-1.,0.)) ;
#11211 = DIRECTION('center_axis',(0.,1.,0.)) ;
#11212 = DIRECTION('ref_axis',(-1.,0.,0.)) ;
#11213 = DIRECTION('',(-1.,0.,0.)) ;
#11214 = DIRECTION('center_axis',(-1.,0.,0.)) ;
#11215 = DIRECTION('ref_axis',(0.,-1.,0.)) ;
#11216 = DIRECTION('',(0.,-1.,0.)) ;
#11217 = DIRECTION('center_axis',(0.,0.,1.)) ;
#11218 = DIRECTION('ref_axis',(1.,0.,0.)) ;
#11219 = DIRECTION('axis',(0.,0.,1.)) ;
#11220 = DIRECTION('refdir',(1.,0.,0.)) ;
#11221 = DIRECTION('center_axis',(0.,1.,0.)) ;
#11222 = DIRECTION('ref_axis',(1.,0.,0.)) ;
#11223 = DIRECTION('center_axis',(0.,1.,0.)) ;
#11224 = DIRECTION('ref_axis',(1.,0.,0.)) ;
#11225 = DIRECTION('',(0.,1.,0.)) ;
#11226 = DIRECTION('center_axis',(0.,-1.,0.)) ;
#11227 = DIRECTION('ref_axis',(1.,0.,0.)) ;
#11228 = DIRECTION('center_axis',(0.,1.,0.)) ;
#11229 = DIRECTION('ref_axis',(1.,0.,0.)) ;
#11230 = DIRECTION('center_axis',(0.,1.,0.)) ;
#11231 = DIRECTION('ref_axis',(1.,0.,0.)) ;
#11232 = DIRECTION('',(0.,1.,0.)) ;
#11233 = DIRECTION('center_axis',(0.,-1.,0.)) ;
#11234 = DIRECTION('ref_axis',(1.,0.,0.)) ;
#11235 = DIRECTION('center_axis',(0.,1.,0.)) ;
#11236 = DIRECTION('ref_axis',(0.,0.,1.)) ;
#11237 = DIRECTION('',(-1.,0.,0.)) ;
#11238 = DIRECTION('',(0.,0.,-1.)) ;
#11239 = DIRECTION('',(-1.,0.,0.)) ;
#11240 = DIRECTION('',(0.,0.,1.)) ;
#11241 = DIRECTION('center_axis',(1.,0.,0.)) ;
#11242 = DIRECTION('ref_axis',(0.,0.,-1.)) ;
#11243 = DIRECTION('',(0.,1.,0.)) ;
#11244 = DIRECTION('',(0.,0.,1.)) ;
#11245 = DIRECTION('',(0.,1.,0.)) ;
#11246 = DIRECTION('',(0.,0.,1.)) ;
#11247 = DIRECTION('',(0.,1.,0.)) ;
#11248 = DIRECTION('center_axis',(-1.,0.,0.)) ;
#11249 = DIRECTION('ref_axis',(0.,0.,1.)) ;
#11250 = DIRECTION('',(0.,-1.,0.)) ;
#11251 = DIRECTION('',(0.,1.,0.)) ;
#11252 = DIRECTION('',(0.,0.,-1.)) ;
#11253 = DIRECTION('center_axis',(0.,0.,-1.)) ;
#11254 = DIRECTION('ref_axis',(-1.,0.,0.)) ;
#11255 = DIRECTION('',(1.,0.,0.)) ;
#11256 = DIRECTION('center_axis',(0.,1.,0.)) ;
#11257 = DIRECTION('ref_axis',(1.,0.,0.)) ;
#11258 = DIRECTION('',(1.,0.,0.)) ;
#11259 = DIRECTION('',(1.,0.,0.)) ;
#11260 = DIRECTION('',(0.,0.,-1.)) ;
#11261 = DIRECTION('center_axis',(0.,0.,1.)) ;
#11262 = DIRECTION('ref_axis',(1.77635683940025E-15,-1.,0.)) ;
#11263 = DIRECTION('center_axis',(0.,0.,1.)) ;
#11264 = DIRECTION('ref_axis',(1.77635683940025E-15,-1.,0.)) ;
#11265 = DIRECTION('',(0.,0.,1.)) ;
#11266 = DIRECTION('center_axis',(0.,0.,1.)) ;
#11267 = DIRECTION('ref_axis',(1.77635683940025E-15,-1.,0.)) ;
#11268 = DIRECTION('center_axis',(0.,0.,1.)) ;
#11269 = DIRECTION('ref_axis',(1.77635683940025E-15,-1.,0.)) ;
#11270 = DIRECTION('center_axis',(0.,0.,1.)) ;
#11271 = DIRECTION('ref_axis',(1.77635683940025E-15,-1.,0.)) ;
#11272 = DIRECTION('',(0.,0.,1.)) ;
#11273 = DIRECTION('center_axis',(0.,0.,1.)) ;
#11274 = DIRECTION('ref_axis',(1.77635683940025E-15,-1.,0.)) ;
#11275 = DIRECTION('center_axis',(0.,0.,1.)) ;
#11276 = DIRECTION('ref_axis',(1.,0.,0.)) ;
#11277 = DIRECTION('center_axis',(0.,0.,1.)) ;
#11278 = DIRECTION('ref_axis',(-1.,-1.48029736616687E-15,0.)) ;
#11279 = DIRECTION('',(0.,-1.,0.)) ;
#11280 = DIRECTION('center_axis',(0.,0.,1.)) ;
#11281 = DIRECTION('ref_axis',(-2.96059473233374E-15,1.,0.)) ;
#11282 = DIRECTION('',(-1.,0.,0.)) ;
#11283 = DIRECTION('center_axis',(0.,0.,1.)) ;
#11284 = DIRECTION('ref_axis',(1.,1.48029736616687E-15,0.)) ;
#11285 = DIRECTION('',(0.,1.,0.)) ;
#11286 = DIRECTION('center_axis',(0.,0.,1.)) ;
#11287 = DIRECTION('ref_axis',(2.96059473233374E-15,-1.,0.)) ;
#11288 = DIRECTION('',(1.,0.,0.)) ;
#11289 = DIRECTION('',(0.,1.,0.)) ;
#11290 = DIRECTION('center_axis',(0.,0.,1.)) ;
#11291 = DIRECTION('ref_axis',(1.,1.77635683940025E-15,0.)) ;
#11292 = DIRECTION('',(0.,1.,0.)) ;
#11293 = DIRECTION('',(-1.,0.,0.)) ;
#11294 = DIRECTION('center_axis',(0.,0.,1.)) ;
#11295 = DIRECTION('ref_axis',(1.,1.77635683940025E-15,0.)) ;
#11296 = DIRECTION('',(-1.,0.,0.)) ;
#11297 = DIRECTION('center_axis',(0.,0.,1.)) ;
#11298 = DIRECTION('ref_axis',(-1.77635683940025E-15,1.,0.)) ;
#11299 = DIRECTION('',(0.,-1.,0.)) ;
#11300 = DIRECTION('center_axis',(0.,0.,1.)) ;
#11301 = DIRECTION('ref_axis',(-1.,-1.77635683940025E-15,0.)) ;
#11302 = DIRECTION('',(1.,0.,0.)) ;
#11303 = DIRECTION('center_axis',(0.,1.,0.)) ;
#11304 = DIRECTION('ref_axis',(1.,0.,0.)) ;
#11305 = DIRECTION('',(1.,0.,0.)) ;
#11306 = DIRECTION('',(0.,0.,-1.)) ;
#11307 = DIRECTION('',(1.,0.,0.)) ;
#11308 = DIRECTION('',(0.,0.,1.)) ;
#11309 = DIRECTION('center_axis',(-1.,0.,0.)) ;
#11310 = DIRECTION('ref_axis',(0.,0.,1.)) ;
#11311 = DIRECTION('',(0.,-1.,0.)) ;
#11312 = DIRECTION('',(0.,0.,1.)) ;
#11313 = DIRECTION('',(0.,1.,0.)) ;
#11314 = DIRECTION('center_axis',(0.,1.,0.)) ;
#11315 = DIRECTION('ref_axis',(0.,0.,1.)) ;
#11316 = DIRECTION('',(-1.,0.,0.)) ;
#11317 = DIRECTION('',(0.,0.,1.)) ;
#11318 = DIRECTION('',(0.,0.,-1.)) ;
#11319 = DIRECTION('',(-1.,0.,0.)) ;
#11320 = DIRECTION('center_axis',(0.,0.,-1.)) ;
#11321 = DIRECTION('ref_axis',(-1.,0.,0.)) ;
#11322 = DIRECTION('',(0.,1.,0.)) ;
#11323 = DIRECTION('center_axis',(1.,0.,0.)) ;
#11324 = DIRECTION('ref_axis',(0.,0.,-1.)) ;
#11325 = DIRECTION('',(0.,1.,0.)) ;
#11326 = DIRECTION('',(0.,0.,-1.)) ;
#11327 = DIRECTION('center_axis',(0.,0.,1.)) ;
#11328 = DIRECTION('ref_axis',(1.,1.77635683940025E-15,0.)) ;
#11329 = DIRECTION('center_axis',(0.,0.,1.)) ;
#11330 = DIRECTION('ref_axis',(1.,1.77635683940025E-15,0.)) ;
#11331 = DIRECTION('',(0.,0.,1.)) ;
#11332 = DIRECTION('center_axis',(0.,0.,1.)) ;
#11333 = DIRECTION('ref_axis',(1.,1.77635683940025E-15,0.)) ;
#11334 = DIRECTION('',(0.,0.,1.)) ;
#11335 = DIRECTION('center_axis',(0.,0.,1.)) ;
#11336 = DIRECTION('ref_axis',(1.,1.77635683940025E-15,0.)) ;
#11337 = DIRECTION('center_axis',(0.,-1.,0.)) ;
#11338 = DIRECTION('ref_axis',(-0.707106781186548,0.,0.707106781186548)) ;
#11339 = DIRECTION('center_axis',(0.,-1.,0.)) ;
#11340 = DIRECTION('ref_axis',(0.,0.,1.)) ;
#11341 = DIRECTION('',(0.,-1.,0.)) ;
#11342 = DIRECTION('center_axis',(0.,1.,0.)) ;
#11343 = DIRECTION('ref_axis',(-1.,0.,0.)) ;
#11344 = DIRECTION('',(0.,1.,0.)) ;
#11345 = DIRECTION('center_axis',(0.,0.,1.)) ;
#11346 = DIRECTION('ref_axis',(1.,0.,0.)) ;
#11347 = DIRECTION('center_axis',(-1.,0.,0.)) ;
#11348 = DIRECTION('ref_axis',(0.,-1.,0.)) ;
#11349 = DIRECTION('center_axis',(0.,0.,-1.)) ;
#11350 = DIRECTION('ref_axis',(-0.707106781186548,-0.707106781186548,0.)) ;
#11351 = DIRECTION('center_axis',(0.,0.,1.)) ;
#11352 = DIRECTION('ref_axis',(-0.707106781186547,-0.707106781186547,0.)) ;
#11353 = DIRECTION('center_axis',(1.,0.,0.)) ;
#11354 = DIRECTION('ref_axis',(0.,-0.70710678118656,0.707106781186535)) ;
#11355 = DIRECTION('center_axis',(-1.,1.77635683940026E-14,0.)) ;
#11356 = DIRECTION('ref_axis',(-1.77635683940026E-14,-1.,0.)) ;
#11357 = DIRECTION('',(-1.,0.,0.)) ;
#11358 = DIRECTION('',(1.,0.,0.)) ;
#11359 = DIRECTION('center_axis',(0.,0.,1.)) ;
#11360 = DIRECTION('ref_axis',(1.,0.,0.)) ;
#11361 = DIRECTION('center_axis',(0.,-1.,0.)) ;
#11362 = DIRECTION('ref_axis',(1.,0.,0.)) ;
#11363 = DIRECTION('center_axis',(0.,0.,-1.)) ;
#11364 = DIRECTION('ref_axis',(0.707106781186548,-0.707106781186548,0.)) ;
#11365 = DIRECTION('center_axis',(0.,0.,1.)) ;
#11366 = DIRECTION('ref_axis',(0.707106781186547,-0.707106781186547,0.)) ;
#11367 = DIRECTION('center_axis',(0.,1.,0.)) ;
#11368 = DIRECTION('ref_axis',(0.707106781186548,0.,0.707106781186548)) ;
#11369 = DIRECTION('center_axis',(0.,-1.,0.)) ;
#11370 = DIRECTION('ref_axis',(1.,0.,0.)) ;
#11371 = DIRECTION('',(0.,-1.,0.)) ;
#11372 = DIRECTION('',(0.,1.,0.)) ;
#11373 = DIRECTION('center_axis',(0.,0.,1.)) ;
#11374 = DIRECTION('ref_axis',(1.,0.,0.)) ;
#11375 = DIRECTION('center_axis',(1.,0.,0.)) ;
#11376 = DIRECTION('ref_axis',(0.,1.,0.)) ;
#11377 = DIRECTION('center_axis',(0.,0.,-1.)) ;
#11378 = DIRECTION('ref_axis',(0.707106781186548,0.707106781186548,0.)) ;
#11379 = DIRECTION('center_axis',(0.,0.,1.)) ;
#11380 = DIRECTION('ref_axis',(0.707106781186547,0.707106781186547,0.)) ;
#11381 = DIRECTION('center_axis',(-1.,0.,0.)) ;
#11382 = DIRECTION('ref_axis',(0.,0.70710678118656,0.707106781186535)) ;
#11383 = DIRECTION('center_axis',(1.,-1.77635683940026E-14,0.)) ;
#11384 = DIRECTION('ref_axis',(1.77635683940026E-14,1.,0.)) ;
#11385 = DIRECTION('',(1.,0.,0.)) ;
#11386 = DIRECTION('',(-1.,0.,0.)) ;
#11387 = DIRECTION('center_axis',(0.,0.,1.)) ;
#11388 = DIRECTION('ref_axis',(1.,0.,0.)) ;
#11389 = DIRECTION('center_axis',(0.,0.,-1.)) ;
#11390 = DIRECTION('ref_axis',(-0.707106781186548,0.707106781186548,0.)) ;
#11391 = DIRECTION('center_axis',(0.,0.,1.)) ;
#11392 = DIRECTION('ref_axis',(-0.707106781186547,0.707106781186547,0.)) ;
#11393 = DIRECTION('center_axis',(0.,0.,1.)) ;
#11394 = DIRECTION('ref_axis',(2.96059473233374E-15,-1.,0.)) ;
#11395 = DIRECTION('',(0.,0.,1.)) ;
#11396 = DIRECTION('',(0.,0.,1.)) ;
#11397 = DIRECTION('center_axis',(0.,-1.,0.)) ;
#11398 = DIRECTION('ref_axis',(1.,0.,0.)) ;
#11399 = DIRECTION('',(0.,0.,1.)) ;
#11400 = DIRECTION('center_axis',(0.,0.,1.)) ;
#11401 = DIRECTION('ref_axis',(-1.,-1.48029736616687E-15,0.)) ;
#11402 = DIRECTION('',(0.,0.,1.)) ;
#11403 = DIRECTION('center_axis',(-1.,0.,0.)) ;
#11404 = DIRECTION('ref_axis',(0.,-1.,0.)) ;
#11405 = DIRECTION('',(0.,0.,1.)) ;
#11406 = DIRECTION('center_axis',(0.,0.,1.)) ;
#11407 = DIRECTION('ref_axis',(1.,0.,0.)) ;
#11408 = DIRECTION('center_axis',(-1.,0.,0.)) ;
#11409 = DIRECTION('ref_axis',(0.,-1.,0.)) ;
#11410 = DIRECTION('',(0.,0.,1.)) ;
#11411 = DIRECTION('',(0.,-1.,0.)) ;
#11412 = DIRECTION('',(0.,0.,1.)) ;
#11413 = DIRECTION('center_axis',(0.,0.,1.)) ;
#11414 = DIRECTION('ref_axis',(-1.77635683940025E-15,1.,0.)) ;
#11415 = DIRECTION('',(0.,0.,1.)) ;
#11416 = DIRECTION('center_axis',(0.,0.,1.)) ;
#11417 = DIRECTION('ref_axis',(-1.77635683940025E-15,1.,0.)) ;
#11418 = DIRECTION('center_axis',(0.,1.,0.)) ;
#11419 = DIRECTION('ref_axis',(-1.,0.,0.)) ;
#11420 = DIRECTION('',(-1.,0.,0.)) ;
#11421 = DIRECTION('center_axis',(1.,0.,0.)) ;
#11422 = DIRECTION('ref_axis',(0.,1.,0.)) ;
#11423 = DIRECTION('',(0.,1.,0.)) ;
#11424 = DIRECTION('center_axis',(0.,-1.,0.)) ;
#11425 = DIRECTION('ref_axis',(1.,0.,0.)) ;
#11426 = DIRECTION('',(0.,0.,1.)) ;
#11427 = DIRECTION('',(1.,0.,0.)) ;
#11428 = DIRECTION('center_axis',(0.,0.,1.)) ;
#11429 = DIRECTION('ref_axis',(-1.,-1.77635683940025E-15,0.)) ;
#11430 = DIRECTION('center_axis',(0.,0.,1.)) ;
#11431 = DIRECTION('ref_axis',(-1.,-1.77635683940025E-15,0.)) ;
#11432 = DIRECTION('center_axis',(0.,0.,1.)) ;
#11433 = DIRECTION('ref_axis',(1.,0.,0.)) ;
#11434 = DIRECTION('center_axis',(0.,0.,1.)) ;
#11435 = DIRECTION('ref_axis',(-2.96059473233374E-15,1.,0.)) ;
#11436 = DIRECTION('',(0.,0.,1.)) ;
#11437 = DIRECTION('center_axis',(0.,1.,0.)) ;
#11438 = DIRECTION('ref_axis',(-1.,0.,0.)) ;
#11439 = DIRECTION('',(0.,0.,1.)) ;
#11440 = DIRECTION('center_axis',(0.,0.,1.)) ;
#11441 = DIRECTION('ref_axis',(1.,1.48029736616687E-15,0.)) ;
#11442 = DIRECTION('',(0.,0.,1.)) ;
#11443 = DIRECTION('center_axis',(1.,0.,0.)) ;
#11444 = DIRECTION('ref_axis',(0.,1.,0.)) ;
#11445 = DIRECTION('axis',(0.,0.,1.)) ;
#11446 = DIRECTION('refdir',(1.,0.,0.)) ;
#11447 = DIRECTION('center_axis',(0.,1.,0.)) ;
#11448 = DIRECTION('ref_axis',(1.,0.,0.)) ;
#11449 = DIRECTION('center_axis',(0.,1.,0.)) ;
#11450 = DIRECTION('ref_axis',(1.,0.,0.)) ;
#11451 = DIRECTION('',(0.,-1.,0.)) ;
#11452 = DIRECTION('center_axis',(0.,-1.,0.)) ;
#11453 = DIRECTION('ref_axis',(1.,0.,0.)) ;
#11454 = DIRECTION('center_axis',(0.,1.,0.)) ;
#11455 = DIRECTION('ref_axis',(1.,0.,0.)) ;
#11456 = DIRECTION('center_axis',(0.,-1.,0.)) ;
#11457 = DIRECTION('ref_axis',(1.,0.,0.)) ;
#11458 = DIRECTION('',(0.,-1.,0.)) ;
#11459 = DIRECTION('center_axis',(0.,-1.,0.)) ;
#11460 = DIRECTION('ref_axis',(1.,0.,0.)) ;
#11461 = DIRECTION('center_axis',(0.,1.,0.)) ;
#11462 = DIRECTION('ref_axis',(1.,0.,0.)) ;
#11463 = DIRECTION('center_axis',(0.,-1.,0.)) ;
#11464 = DIRECTION('ref_axis',(1.,0.,0.)) ;
#11465 = DIRECTION('',(0.,-1.,0.)) ;
#11466 = DIRECTION('center_axis',(0.,-1.,0.)) ;
#11467 = DIRECTION('ref_axis',(1.,0.,0.)) ;
#11468 = DIRECTION('center_axis',(0.,1.,0.)) ;
#11469 = DIRECTION('ref_axis',(1.,0.,0.)) ;
#11470 = DIRECTION('center_axis',(0.,-1.,0.)) ;
#11471 = DIRECTION('ref_axis',(1.,0.,0.)) ;
#11472 = DIRECTION('',(0.,-1.,0.)) ;
#11473 = DIRECTION('center_axis',(0.,-1.,0.)) ;
#11474 = DIRECTION('ref_axis',(1.,0.,0.)) ;
#11475 = DIRECTION('center_axis',(0.0648275862068965,0.,0.997896479634329)) ;
#11476 = DIRECTION('ref_axis',(0.997896479634329,0.,-0.0648275862068965)) ;
#11477 = DIRECTION('',(0.997896479634329,0.,-0.0648275862068965)) ;
#11478 = DIRECTION('',(0.,1.,0.)) ;
#11479 = DIRECTION('',(0.997896479634329,0.,-0.0648275862068965)) ;
#11480 = DIRECTION('',(0.,1.,0.)) ;
#11481 = DIRECTION('center_axis',(0.,1.,0.)) ;
#11482 = DIRECTION('ref_axis',(-0.0648275862068983,0.,-0.997896479634329)) ;
#11483 = DIRECTION('center_axis',(0.,1.,0.)) ;
#11484 = DIRECTION('ref_axis',(-0.0648275862068983,0.,-0.997896479634329)) ;
#11485 = DIRECTION('center_axis',(0.,1.,0.)) ;
#11486 = DIRECTION('ref_axis',(-0.0648275862068983,0.,-0.997896479634329)) ;
#11487 = DIRECTION('',(0.,1.,0.)) ;
#11488 = DIRECTION('center_axis',(-0.0648275862068965,0.,-0.997896479634329)) ;
#11489 = DIRECTION('ref_axis',(-0.997896479634329,0.,0.0648275862068965)) ;
#11490 = DIRECTION('',(-0.997896479634329,0.,0.0648275862068965)) ;
#11491 = DIRECTION('',(-0.997896479634329,0.,0.0648275862068965)) ;
#11492 = DIRECTION('',(0.,1.,0.)) ;
#11493 = DIRECTION('center_axis',(0.,1.,0.)) ;
#11494 = DIRECTION('ref_axis',(0.064827586206896,0.,0.997896479634329)) ;
#11495 = DIRECTION('center_axis',(0.,1.,0.)) ;
#11496 = DIRECTION('ref_axis',(0.064827586206896,0.,0.997896479634329)) ;
#11497 = DIRECTION('center_axis',(0.,1.,0.)) ;
#11498 = DIRECTION('ref_axis',(0.064827586206896,0.,0.997896479634329)) ;
#11499 = DIRECTION('center_axis',(0.,1.,0.)) ;
#11500 = DIRECTION('ref_axis',(1.,0.,0.)) ;
#11501 = DIRECTION('center_axis',(0.,1.,0.)) ;
#11502 = DIRECTION('ref_axis',(1.,0.,0.)) ;
#11503 = DIRECTION('center_axis',(0.,1.,0.)) ;
#11504 = DIRECTION('ref_axis',(1.,0.,0.)) ;
#11505 = DIRECTION('center_axis',(0.,-1.,0.)) ;
#11506 = DIRECTION('ref_axis',(1.,0.,0.)) ;
#11507 = DIRECTION('',(0.,-1.,0.)) ;
#11508 = DIRECTION('center_axis',(0.,-1.,0.)) ;
#11509 = DIRECTION('ref_axis',(1.,0.,0.)) ;
#11510 = DIRECTION('center_axis',(0.,1.,0.)) ;
#11511 = DIRECTION('ref_axis',(1.,0.,0.)) ;
#11512 = DIRECTION('center_axis',(0.,-1.,0.)) ;
#11513 = DIRECTION('ref_axis',(1.,0.,0.)) ;
#11514 = DIRECTION('',(0.,-1.,0.)) ;
#11515 = DIRECTION('center_axis',(0.,-1.,0.)) ;
#11516 = DIRECTION('ref_axis',(1.,0.,0.)) ;
#11517 = DIRECTION('center_axis',(0.,1.,0.)) ;
#11518 = DIRECTION('ref_axis',(1.,0.,0.)) ;
#11519 = DIRECTION('center_axis',(0.,-1.,0.)) ;
#11520 = DIRECTION('ref_axis',(1.,0.,0.)) ;
#11521 = DIRECTION('',(0.,-1.,0.)) ;
#11522 = DIRECTION('center_axis',(0.,-1.,0.)) ;
#11523 = DIRECTION('ref_axis',(1.,0.,0.)) ;
#11524 = DIRECTION('center_axis',(0.0648275862068965,0.,0.997896479634329)) ;
#11525 = DIRECTION('ref_axis',(0.997896479634329,0.,-0.0648275862068965)) ;
#11526 = DIRECTION('',(0.997896479634329,0.,-0.0648275862068965)) ;
#11527 = DIRECTION('',(0.,1.,0.)) ;
#11528 = DIRECTION('',(0.997896479634329,0.,-0.0648275862068965)) ;
#11529 = DIRECTION('',(0.,1.,0.)) ;
#11530 = DIRECTION('center_axis',(0.,1.,0.)) ;
#11531 = DIRECTION('ref_axis',(-0.0648275862068983,0.,-0.997896479634329)) ;
#11532 = DIRECTION('center_axis',(0.,1.,0.)) ;
#11533 = DIRECTION('ref_axis',(-0.0648275862068983,0.,-0.997896479634329)) ;
#11534 = DIRECTION('center_axis',(0.,1.,0.)) ;
#11535 = DIRECTION('ref_axis',(-0.0648275862068983,0.,-0.997896479634329)) ;
#11536 = DIRECTION('',(0.,1.,0.)) ;
#11537 = DIRECTION('center_axis',(-0.0648275862068965,0.,-0.997896479634329)) ;
#11538 = DIRECTION('ref_axis',(-0.997896479634329,0.,0.0648275862068965)) ;
#11539 = DIRECTION('',(-0.997896479634329,0.,0.0648275862068965)) ;
#11540 = DIRECTION('',(-0.997896479634329,0.,0.0648275862068965)) ;
#11541 = DIRECTION('',(0.,1.,0.)) ;
#11542 = DIRECTION('center_axis',(0.,1.,0.)) ;
#11543 = DIRECTION('ref_axis',(0.064827586206896,0.,0.997896479634329)) ;
#11544 = DIRECTION('center_axis',(0.,1.,0.)) ;
#11545 = DIRECTION('ref_axis',(0.064827586206896,0.,0.997896479634329)) ;
#11546 = DIRECTION('center_axis',(0.,1.,0.)) ;
#11547 = DIRECTION('ref_axis',(0.064827586206896,0.,0.997896479634329)) ;
#11548 = DIRECTION('center_axis',(0.,1.,0.)) ;
#11549 = DIRECTION('ref_axis',(1.,0.,0.)) ;
#11550 = DIRECTION('center_axis',(0.,1.,0.)) ;
#11551 = DIRECTION('ref_axis',(1.,0.,0.)) ;
#11552 = DIRECTION('axis',(0.,0.,1.)) ;
#11553 = DIRECTION('refdir',(1.,0.,0.)) ;
#11554 = DIRECTION('center_axis',(0.,1.,0.)) ;
#11555 = DIRECTION('ref_axis',(1.,0.,0.)) ;
#11556 = DIRECTION('center_axis',(0.,1.,0.)) ;
#11557 = DIRECTION('ref_axis',(1.,0.,0.)) ;
#11558 = DIRECTION('',(0.,-1.,0.)) ;
#11559 = DIRECTION('center_axis',(0.,-1.,0.)) ;
#11560 = DIRECTION('ref_axis',(1.,0.,0.)) ;
#11561 = DIRECTION('center_axis',(0.,1.,0.)) ;
#11562 = DIRECTION('ref_axis',(1.,0.,0.)) ;
#11563 = DIRECTION('center_axis',(0.,1.,0.)) ;
#11564 = DIRECTION('ref_axis',(1.,0.,0.)) ;
#11565 = DIRECTION('',(0.,-1.,0.)) ;
#11566 = DIRECTION('center_axis',(0.,-1.,0.)) ;
#11567 = DIRECTION('ref_axis',(1.,0.,0.)) ;
#11568 = DIRECTION('center_axis',(0.,1.,0.)) ;
#11569 = DIRECTION('ref_axis',(1.,0.,0.)) ;
#11570 = DIRECTION('center_axis',(0.,-1.,0.)) ;
#11571 = DIRECTION('ref_axis',(1.,0.,0.)) ;
#11572 = DIRECTION('',(0.,-1.,0.)) ;
#11573 = DIRECTION('center_axis',(0.,-1.,0.)) ;
#11574 = DIRECTION('ref_axis',(1.,0.,0.)) ;
#11575 = DIRECTION('center_axis',(0.,1.,0.)) ;
#11576 = DIRECTION('ref_axis',(1.,0.,0.)) ;
#11577 = DIRECTION('center_axis',(0.,-1.,0.)) ;
#11578 = DIRECTION('ref_axis',(1.,0.,0.)) ;
#11579 = DIRECTION('',(0.,-1.,0.)) ;
#11580 = DIRECTION('center_axis',(0.,-1.,0.)) ;
#11581 = DIRECTION('ref_axis',(1.,0.,0.)) ;
#11582 = DIRECTION('center_axis',(0.,1.,0.)) ;
#11583 = DIRECTION('ref_axis',(1.,0.,0.)) ;
#11584 = DIRECTION('center_axis',(0.,-1.,0.)) ;
#11585 = DIRECTION('ref_axis',(1.,0.,0.)) ;
#11586 = DIRECTION('',(0.,-1.,0.)) ;
#11587 = DIRECTION('center_axis',(0.,-1.,0.)) ;
#11588 = DIRECTION('ref_axis',(1.,0.,0.)) ;
#11589 = DIRECTION('center_axis',(-0.0648275862068965,0.,0.997896479634329)) ;
#11590 = DIRECTION('ref_axis',(0.997896479634329,0.,0.0648275862068965)) ;
#11591 = DIRECTION('',(0.997896479634329,0.,0.0648275862068965)) ;
#11592 = DIRECTION('',(0.,1.,0.)) ;
#11593 = DIRECTION('',(0.997896479634329,0.,0.0648275862068965)) ;
#11594 = DIRECTION('',(0.,1.,0.)) ;
#11595 = DIRECTION('center_axis',(0.,1.,0.)) ;
#11596 = DIRECTION('ref_axis',(0.0648275862068983,0.,-0.997896479634329)) ;
#11597 = DIRECTION('center_axis',(0.,1.,0.)) ;
#11598 = DIRECTION('ref_axis',(0.0648275862068983,0.,-0.997896479634329)) ;
#11599 = DIRECTION('center_axis',(0.,1.,0.)) ;
#11600 = DIRECTION('ref_axis',(0.0648275862068983,0.,-0.997896479634329)) ;
#11601 = DIRECTION('',(0.,1.,0.)) ;
#11602 = DIRECTION('center_axis',(0.0648275862068965,0.,-0.997896479634329)) ;
#11603 = DIRECTION('ref_axis',(-0.997896479634329,0.,-0.0648275862068965)) ;
#11604 = DIRECTION('',(-0.997896479634329,0.,-0.0648275862068965)) ;
#11605 = DIRECTION('',(-0.997896479634329,0.,-0.0648275862068965)) ;
#11606 = DIRECTION('',(0.,1.,0.)) ;
#11607 = DIRECTION('center_axis',(0.,1.,0.)) ;
#11608 = DIRECTION('ref_axis',(-0.0648275862069006,0.,0.997896479634329)) ;
#11609 = DIRECTION('center_axis',(0.,1.,0.)) ;
#11610 = DIRECTION('ref_axis',(-0.0648275862069006,0.,0.997896479634329)) ;
#11611 = DIRECTION('center_axis',(0.,1.,0.)) ;
#11612 = DIRECTION('ref_axis',(-0.0648275862069006,0.,0.997896479634329)) ;
#11613 = DIRECTION('center_axis',(0.,1.,0.)) ;
#11614 = DIRECTION('ref_axis',(1.,0.,0.)) ;
#11615 = DIRECTION('center_axis',(0.,1.,0.)) ;
#11616 = DIRECTION('ref_axis',(1.,0.,0.)) ;
#11617 = DIRECTION('center_axis',(0.,1.,0.)) ;
#11618 = DIRECTION('ref_axis',(1.,0.,0.)) ;
#11619 = DIRECTION('center_axis',(0.,-1.,0.)) ;
#11620 = DIRECTION('ref_axis',(1.,0.,0.)) ;
#11621 = DIRECTION('',(0.,-1.,0.)) ;
#11622 = DIRECTION('center_axis',(0.,-1.,0.)) ;
#11623 = DIRECTION('ref_axis',(1.,0.,0.)) ;
#11624 = DIRECTION('center_axis',(0.,1.,0.)) ;
#11625 = DIRECTION('ref_axis',(1.,0.,0.)) ;
#11626 = DIRECTION('center_axis',(0.,-1.,0.)) ;
#11627 = DIRECTION('ref_axis',(1.,0.,0.)) ;
#11628 = DIRECTION('',(0.,-1.,0.)) ;
#11629 = DIRECTION('center_axis',(0.,-1.,0.)) ;
#11630 = DIRECTION('ref_axis',(1.,0.,0.)) ;
#11631 = DIRECTION('center_axis',(0.,1.,0.)) ;
#11632 = DIRECTION('ref_axis',(1.,0.,0.)) ;
#11633 = DIRECTION('center_axis',(0.,-1.,0.)) ;
#11634 = DIRECTION('ref_axis',(1.,0.,0.)) ;
#11635 = DIRECTION('',(0.,-1.,0.)) ;
#11636 = DIRECTION('center_axis',(0.,-1.,0.)) ;
#11637 = DIRECTION('ref_axis',(1.,0.,0.)) ;
#11638 = DIRECTION('center_axis',(-0.0648275862068965,0.,0.997896479634329)) ;
#11639 = DIRECTION('ref_axis',(0.997896479634329,0.,0.0648275862068965)) ;
#11640 = DIRECTION('',(0.997896479634329,0.,0.0648275862068965)) ;
#11641 = DIRECTION('',(0.,1.,0.)) ;
#11642 = DIRECTION('',(0.997896479634329,0.,0.0648275862068965)) ;
#11643 = DIRECTION('',(0.,1.,0.)) ;
#11644 = DIRECTION('center_axis',(0.,1.,0.)) ;
#11645 = DIRECTION('ref_axis',(0.0648275862068983,0.,-0.997896479634329)) ;
#11646 = DIRECTION('center_axis',(0.,1.,0.)) ;
#11647 = DIRECTION('ref_axis',(0.0648275862068983,0.,-0.997896479634329)) ;
#11648 = DIRECTION('center_axis',(0.,1.,0.)) ;
#11649 = DIRECTION('ref_axis',(0.0648275862068983,0.,-0.997896479634329)) ;
#11650 = DIRECTION('',(0.,1.,0.)) ;
#11651 = DIRECTION('center_axis',(0.0648275862068965,0.,-0.997896479634329)) ;
#11652 = DIRECTION('ref_axis',(-0.997896479634329,0.,-0.0648275862068965)) ;
#11653 = DIRECTION('',(-0.997896479634329,0.,-0.0648275862068965)) ;
#11654 = DIRECTION('',(-0.997896479634329,0.,-0.0648275862068965)) ;
#11655 = DIRECTION('',(0.,1.,0.)) ;
#11656 = DIRECTION('center_axis',(0.,1.,0.)) ;
#11657 = DIRECTION('ref_axis',(-0.0648275862069006,0.,0.997896479634329)) ;
#11658 = DIRECTION('center_axis',(0.,1.,0.)) ;
#11659 = DIRECTION('ref_axis',(-0.0648275862069006,0.,0.997896479634329)) ;
#11660 = DIRECTION('center_axis',(0.,1.,0.)) ;
#11661 = DIRECTION('ref_axis',(-0.0648275862069006,0.,0.997896479634329)) ;
#11662 = DIRECTION('center_axis',(0.,1.,0.)) ;
#11663 = DIRECTION('ref_axis',(1.,0.,0.)) ;
#11664 = DIRECTION('center_axis',(0.,1.,0.)) ;
#11665 = DIRECTION('ref_axis',(1.,0.,0.)) ;
#11666 = DIRECTION('axis',(0.,0.,1.)) ;
#11667 = DIRECTION('refdir',(1.,0.,0.)) ;
#11668 = DIRECTION('center_axis',(0.,1.,0.)) ;
#11669 = DIRECTION('ref_axis',(1.,0.,0.)) ;
#11670 = DIRECTION('',(0.,-1.,0.)) ;
#11671 = DIRECTION('center_axis',(0.,1.,0.)) ;
#11672 = DIRECTION('ref_axis',(1.,0.,0.)) ;
#11673 = DIRECTION('center_axis',(0.,1.,0.)) ;
#11674 = DIRECTION('ref_axis',(1.,0.,0.)) ;
#11675 = DIRECTION('',(0.,-1.,0.)) ;
#11676 = DIRECTION('center_axis',(0.,1.,0.)) ;
#11677 = DIRECTION('ref_axis',(1.,0.,0.)) ;
#11678 = DIRECTION('center_axis',(0.,1.,0.)) ;
#11679 = DIRECTION('ref_axis',(1.,0.,0.)) ;
#11680 = DIRECTION('center_axis',(0.,1.,0.)) ;
#11681 = DIRECTION('ref_axis',(1.,0.,0.)) ;
#11682 = DIRECTION('center_axis',(0.,1.,0.)) ;
#11683 = DIRECTION('ref_axis',(1.,0.,0.)) ;
#11684 = DIRECTION('',(0.,1.,0.)) ;
#11685 = DIRECTION('center_axis',(0.,-1.,0.)) ;
#11686 = DIRECTION('ref_axis',(1.,0.,0.)) ;
#11687 = DIRECTION('center_axis',(-0.993765553407216,0.,0.11149002135281)) ;
#11688 = DIRECTION('ref_axis',(0.11149002135281,0.,0.993765553407216)) ;
#11689 = DIRECTION('center_axis',(0.993765553407216,0.,-0.11149002135281)) ;
#11690 = DIRECTION('ref_axis',(0.11149002135281,0.,0.993765553407216)) ;
#11691 = DIRECTION('center_axis',(0.993765553407216,0.,-0.11149002135281)) ;
#11692 = DIRECTION('ref_axis',(-0.111490021352808,0.,-0.993765553407216)) ;
#11693 = DIRECTION('',(-0.993765553407216,0.,0.11149002135281)) ;
#11694 = DIRECTION('center_axis',(0.993765553407216,0.,-0.11149002135281)) ;
#11695 = DIRECTION('ref_axis',(0.11149002135281,0.,0.993765553407216)) ;
#11696 = DIRECTION('center_axis',(0.993765553407216,0.,-0.11149002135281)) ;
#11697 = DIRECTION('ref_axis',(-0.11149002135281,0.,-0.993765553407216)) ;
#11698 = DIRECTION('center_axis',(0.993765553407216,0.,-0.11149002135281)) ;
#11699 = DIRECTION('ref_axis',(0.11149002135281,0.,0.993765553407216)) ;
#11700 = DIRECTION('center_axis',(0.993765553407216,0.,-0.11149002135281)) ;
#11701 = DIRECTION('ref_axis',(-0.111490021352808,0.,-0.993765553407216)) ;
#11702 = DIRECTION('',(-0.993765553407216,0.,0.11149002135281)) ;
#11703 = DIRECTION('center_axis',(0.993765553407216,0.,-0.11149002135281)) ;
#11704 = DIRECTION('ref_axis',(0.11149002135281,0.,0.993765553407216)) ;
#11705 = DIRECTION('center_axis',(-0.993765553407216,0.,0.11149002135281)) ;
#11706 = DIRECTION('ref_axis',(0.11149002135281,0.,0.993765553407216)) ;
#11707 = DIRECTION('center_axis',(0.993765553407216,0.,-0.11149002135281)) ;
#11708 = DIRECTION('ref_axis',(0.11149002135281,0.,0.993765553407216)) ;
#11709 = DIRECTION('center_axis',(0.993765553407216,0.,-0.11149002135281)) ;
#11710 = DIRECTION('ref_axis',(-0.111490021352808,0.,-0.993765553407216)) ;
#11711 = DIRECTION('center_axis',(0.993765553407216,0.,-0.11149002135281)) ;
#11712 = DIRECTION('ref_axis',(0.11149002135281,0.,0.993765553407216)) ;
#11713 = DIRECTION('',(-0.993765553407216,0.,0.11149002135281)) ;
#11714 = DIRECTION('center_axis',(0.993765553407216,0.,-0.11149002135281)) ;
#11715 = DIRECTION('ref_axis',(-0.11149002135281,0.,-0.993765553407216)) ;
#11716 = DIRECTION('center_axis',(0.993765553407216,0.,-0.11149002135281)) ;
#11717 = DIRECTION('ref_axis',(0.11149002135281,0.,0.993765553407216)) ;
#11718 = DIRECTION('center_axis',(0.993765553407216,0.,-0.11149002135281)) ;
#11719 = DIRECTION('ref_axis',(-0.111490021352808,0.,-0.993765553407216)) ;
#11720 = DIRECTION('',(-0.993765553407216,0.,0.11149002135281)) ;
#11721 = DIRECTION('center_axis',(0.,1.,0.)) ;
#11722 = DIRECTION('ref_axis',(1.,0.,0.)) ;
#11723 = DIRECTION('center_axis',(0.,1.,0.)) ;
#11724 = DIRECTION('ref_axis',(1.,0.,0.)) ;
#11725 = DIRECTION('center_axis',(0.,1.,0.)) ;
#11726 = DIRECTION('ref_axis',(1.,0.,0.)) ;
#11727 = DIRECTION('center_axis',(0.,1.,0.)) ;
#11728 = DIRECTION('ref_axis',(1.,0.,0.)) ;
#11729 = DIRECTION('axis',(0.,0.,1.)) ;
#11730 = DIRECTION('refdir',(1.,0.,0.)) ;
#11731 = DIRECTION('center_axis',(0.,1.,0.)) ;
#11732 = DIRECTION('ref_axis',(1.,0.,0.)) ;
#11733 = DIRECTION('',(0.,-1.,0.)) ;
#11734 = DIRECTION('center_axis',(0.,1.,0.)) ;
#11735 = DIRECTION('ref_axis',(1.,0.,0.)) ;
#11736 = DIRECTION('',(0.,1.,0.)) ;
#11737 = DIRECTION('center_axis',(0.,1.,0.)) ;
#11738 = DIRECTION('ref_axis',(1.,0.,0.)) ;
#11739 = DIRECTION('center_axis',(0.,1.,0.)) ;
#11740 = DIRECTION('ref_axis',(1.,0.,0.)) ;
#11741 = DIRECTION('center_axis',(0.,1.,0.)) ;
#11742 = DIRECTION('ref_axis',(1.,0.,0.)) ;
#11743 = DIRECTION('',(0.,1.,0.)) ;
#11744 = DIRECTION('center_axis',(0.,-1.,0.)) ;
#11745 = DIRECTION('ref_axis',(1.,0.,0.)) ;
#11746 = DIRECTION('center_axis',(0.,1.,0.)) ;
#11747 = DIRECTION('ref_axis',(1.,0.,0.)) ;
#11748 = DIRECTION('center_axis',(0.,1.,0.)) ;
#11749 = DIRECTION('ref_axis',(1.,0.,0.)) ;
#11750 = DIRECTION('',(0.,-1.,0.)) ;
#11751 = DIRECTION('center_axis',(0.,1.,0.)) ;
#11752 = DIRECTION('ref_axis',(1.,0.,0.)) ;
#11753 = DIRECTION('center_axis',(0.,1.,0.)) ;
#11754 = DIRECTION('ref_axis',(1.,0.,0.)) ;
#11755 = DIRECTION('center_axis',(0.,1.,0.)) ;
#11756 = DIRECTION('ref_axis',(1.,0.,0.)) ;
#11757 = DIRECTION('center_axis',(-0.993765553407216,0.,0.11149002135281)) ;
#11758 = DIRECTION('ref_axis',(0.11149002135281,0.,0.993765553407216)) ;
#11759 = DIRECTION('center_axis',(0.993765553407216,0.,-0.11149002135281)) ;
#11760 = DIRECTION('ref_axis',(0.11149002135281,0.,0.993765553407216)) ;
#11761 = DIRECTION('center_axis',(0.993765553407216,0.,-0.11149002135281)) ;
#11762 = DIRECTION('ref_axis',(0.11149002135281,0.,0.993765553407216)) ;
#11763 = DIRECTION('center_axis',(-0.993765553407216,0.,0.11149002135281)) ;
#11764 = DIRECTION('ref_axis',(0.11149002135281,0.,0.993765553407216)) ;
#11765 = DIRECTION('center_axis',(0.993765553407216,0.,-0.11149002135281)) ;
#11766 = DIRECTION('ref_axis',(0.11149002135281,0.,0.993765553407216)) ;
#11767 = DIRECTION('center_axis',(0.993765553407216,0.,-0.11149002135281)) ;
#11768 = DIRECTION('ref_axis',(-0.111490021352811,0.,-0.993765553407216)) ;
#11769 = DIRECTION('center_axis',(0.993765553407216,0.,-0.11149002135281)) ;
#11770 = DIRECTION('ref_axis',(0.11149002135281,0.,0.993765553407216)) ;
#11771 = DIRECTION('',(-0.993765553407216,0.,0.11149002135281)) ;
#11772 = DIRECTION('center_axis',(-0.993765553407216,0.,0.11149002135281)) ;
#11773 = DIRECTION('ref_axis',(0.11149002135281,0.,0.993765553407216)) ;
#11774 = DIRECTION('center_axis',(0.993765553407216,0.,-0.11149002135281)) ;
#11775 = DIRECTION('ref_axis',(0.11149002135281,0.,0.993765553407216)) ;
#11776 = DIRECTION('center_axis',(0.993765553407216,0.,-0.11149002135281)) ;
#11777 = DIRECTION('ref_axis',(-0.111490021352811,0.,-0.993765553407216)) ;
#11778 = DIRECTION('center_axis',(0.993765553407216,0.,-0.11149002135281)) ;
#11779 = DIRECTION('ref_axis',(0.11149002135281,0.,0.993765553407216)) ;
#11780 = DIRECTION('',(-0.993765553407216,0.,0.11149002135281)) ;
#11781 = DIRECTION('center_axis',(0.993765553407216,0.,-0.11149002135281)) ;
#11782 = DIRECTION('ref_axis',(-0.11149002135281,0.,-0.993765553407216)) ;
#11783 = DIRECTION('axis',(0.,0.,1.)) ;
#11784 = DIRECTION('refdir',(1.,0.,0.)) ;
#11785 = DIRECTION('center_axis',(0.,1.,0.)) ;
#11786 = DIRECTION('ref_axis',(-1.,0.,1.22464679914735E-16)) ;
#11787 = DIRECTION('',(0.,1.,0.)) ;
#11788 = DIRECTION('center_axis',(0.,1.,0.)) ;
#11789 = DIRECTION('ref_axis',(1.,0.,0.)) ;
#11790 = DIRECTION('',(0.,-1.,0.)) ;
#11791 = DIRECTION('center_axis',(0.,-1.,0.)) ;
#11792 = DIRECTION('ref_axis',(1.,0.,0.)) ;
#11793 = DIRECTION('center_axis',(0.,1.,0.)) ;
#11794 = DIRECTION('ref_axis',(1.,0.,0.)) ;
#11795 = DIRECTION('',(0.,0.,1.)) ;
#11796 = DIRECTION('',(-1.,0.,0.)) ;
#11797 = DIRECTION('',(0.,0.,-1.)) ;
#11798 = DIRECTION('',(-1.,0.,0.)) ;
#11799 = DIRECTION('',(0.,0.,1.)) ;
#11800 = DIRECTION('',(1.,0.,0.)) ;
#11801 = DIRECTION('',(0.,0.,1.)) ;
#11802 = DIRECTION('center_axis',(1.,0.,0.)) ;
#11803 = DIRECTION('ref_axis',(0.,0.,-1.)) ;
#11804 = DIRECTION('',(0.,0.,-1.)) ;
#11805 = DIRECTION('',(0.,1.,0.)) ;
#11806 = DIRECTION('center_axis',(1.,0.,0.)) ;
#11807 = DIRECTION('ref_axis',(0.,0.,-1.)) ;
#11808 = DIRECTION('',(0.,1.,0.)) ;
#11809 = DIRECTION('',(0.,0.,-1.)) ;
#11810 = DIRECTION('center_axis',(0.,0.,-1.)) ;
#11811 = DIRECTION('ref_axis',(-1.,0.,0.)) ;
#11812 = DIRECTION('center_axis',(0.,0.,-1.)) ;
#11813 = DIRECTION('ref_axis',(1.,0.,0.)) ;
#11814 = DIRECTION('',(0.,1.,0.)) ;
#11815 = DIRECTION('',(-1.,0.,0.)) ;
#11816 = DIRECTION('center_axis',(0.,0.,-1.)) ;
#11817 = DIRECTION('ref_axis',(-1.,0.,0.)) ;
#11818 = DIRECTION('center_axis',(0.,0.,-1.)) ;
#11819 = DIRECTION('ref_axis',(1.,0.,0.)) ;
#11820 = DIRECTION('',(-1.,0.,0.)) ;
#11821 = DIRECTION('center_axis',(-1.,0.,0.)) ;
#11822 = DIRECTION('ref_axis',(0.,0.,1.)) ;
#11823 = DIRECTION('',(0.,1.,0.)) ;
#11824 = DIRECTION('',(0.,1.,0.)) ;
#11825 = DIRECTION('',(0.,0.,1.)) ;
#11826 = DIRECTION('',(0.,0.,-1.)) ;
#11827 = DIRECTION('center_axis',(0.,0.,1.)) ;
#11828 = DIRECTION('ref_axis',(1.,0.,0.)) ;
#11829 = DIRECTION('',(1.,0.,0.)) ;
#11830 = DIRECTION('center_axis',(0.,1.,0.)) ;
#11831 = DIRECTION('ref_axis',(0.,0.,1.)) ;
#11832 = DIRECTION('center_axis',(0.,0.,1.)) ;
#11833 = DIRECTION('ref_axis',(1.,0.,0.)) ;
#11834 = DIRECTION('center_axis',(0.,0.,1.)) ;
#11835 = DIRECTION('ref_axis',(1.,0.,0.)) ;
#11836 = DIRECTION('center_axis',(0.,0.,-1.)) ;
#11837 = DIRECTION('ref_axis',(-0.338432122698804,-0.940990806716825,0.)) ;
#11838 = DIRECTION('center_axis',(0.,0.,1.)) ;
#11839 = DIRECTION('ref_axis',(1.,0.,0.)) ;
#11840 = DIRECTION('center_axis',(0.,0.,1.)) ;
#11841 = DIRECTION('ref_axis',(1.,0.,0.)) ;
#11842 = DIRECTION('center_axis',(0.,0.,-1.)) ;
#11843 = DIRECTION('ref_axis',(-1.,0.,0.)) ;
#11844 = DIRECTION('',(0.,-1.,0.)) ;
#11845 = DIRECTION('center_axis',(0.,0.,1.)) ;
#11846 = DIRECTION('ref_axis',(1.,0.,0.)) ;
#11847 = DIRECTION('center_axis',(0.,0.,1.)) ;
#11848 = DIRECTION('ref_axis',(1.,0.,0.)) ;
#11849 = DIRECTION('',(0.,0.,-1.)) ;
#11850 = DIRECTION('center_axis',(0.,0.,-1.)) ;
#11851 = DIRECTION('ref_axis',(1.,0.,0.)) ;
#11852 = DIRECTION('',(0.,0.,1.)) ;
#11853 = DIRECTION('',(0.,0.,-1.)) ;
#11854 = DIRECTION('center_axis',(0.,0.,-1.)) ;
#11855 = DIRECTION('ref_axis',(1.,0.,0.)) ;
#11856 = DIRECTION('center_axis',(0.,0.,1.)) ;
#11857 = DIRECTION('ref_axis',(1.,0.,0.)) ;
#11858 = DIRECTION('',(0.,1.,0.)) ;
#11859 = DIRECTION('',(-1.,0.,0.)) ;
#11860 = DIRECTION('',(0.,-1.,0.)) ;
#11861 = DIRECTION('',(1.,0.,0.)) ;
#11862 = DIRECTION('',(0.,1.,0.)) ;
#11863 = DIRECTION('center_axis',(0.,1.,0.)) ;
#11864 = DIRECTION('ref_axis',(-1.,0.,0.)) ;
#11865 = DIRECTION('',(-1.,0.,0.)) ;
#11866 = DIRECTION('',(0.,0.,1.)) ;
#11867 = DIRECTION('',(0.,0.,1.)) ;
#11868 = DIRECTION('center_axis',(1.,0.,0.)) ;
#11869 = DIRECTION('ref_axis',(0.,1.,0.)) ;
#11870 = DIRECTION('',(0.,0.,1.)) ;
#11871 = DIRECTION('',(0.,1.,0.)) ;
#11872 = DIRECTION('center_axis',(0.,-1.,0.)) ;
#11873 = DIRECTION('ref_axis',(1.,0.,0.)) ;
#11874 = DIRECTION('',(1.,0.,0.)) ;
#11875 = DIRECTION('',(0.,0.,1.)) ;
#11876 = DIRECTION('center_axis',(-1.,0.,0.)) ;
#11877 = DIRECTION('ref_axis',(0.,-1.,0.)) ;
#11878 = DIRECTION('',(0.,-1.,0.)) ;
#11879 = DIRECTION('center_axis',(0.,0.,1.)) ;
#11880 = DIRECTION('ref_axis',(1.,0.,0.)) ;
#11881 = DIRECTION('axis',(0.,0.,1.)) ;
#11882 = DIRECTION('refdir',(1.,0.,0.)) ;
#11883 = DIRECTION('center_axis',(0.,1.,0.)) ;
#11884 = DIRECTION('ref_axis',(-1.,0.,0.)) ;
#11885 = DIRECTION('',(-1.,0.,0.)) ;
#11886 = DIRECTION('',(0.,0.,1.)) ;
#11887 = DIRECTION('',(-1.,0.,0.)) ;
#11888 = DIRECTION('',(0.,0.,1.)) ;
#11889 = DIRECTION('center_axis',(1.,0.,0.)) ;
#11890 = DIRECTION('ref_axis',(0.,1.,0.)) ;
#11891 = DIRECTION('',(0.,1.,0.)) ;
#11892 = DIRECTION('',(0.,1.,0.)) ;
#11893 = DIRECTION('',(0.,0.,1.)) ;
#11894 = DIRECTION('center_axis',(-1.,0.,0.)) ;
#11895 = DIRECTION('ref_axis',(0.,-1.,0.)) ;
#11896 = DIRECTION('',(0.,-1.,0.)) ;
#11897 = DIRECTION('',(0.,0.,1.)) ;
#11898 = DIRECTION('',(0.,-1.,0.)) ;
#11899 = DIRECTION('center_axis',(0.,0.,1.)) ;
#11900 = DIRECTION('ref_axis',(1.,0.,0.)) ;
#11901 = DIRECTION('',(0.,1.,0.)) ;
#11902 = DIRECTION('',(1.,0.,0.)) ;
#11903 = DIRECTION('',(1.,0.,0.)) ;
#11904 = DIRECTION('',(0.,-1.,0.)) ;
#11905 = DIRECTION('',(-1.,0.,0.)) ;
#11906 = DIRECTION('center_axis',(0.,0.,1.)) ;
#11907 = DIRECTION('ref_axis',(1.,0.,0.)) ;
#11908 = DIRECTION('',(1.,0.,0.)) ;
#11909 = DIRECTION('center_axis',(0.,1.,0.)) ;
#11910 = DIRECTION('ref_axis',(1.,0.,0.)) ;
#11911 = DIRECTION('',(-0.52999894000318,0.,0.847998304005088)) ;
#11912 = DIRECTION('center_axis',(0.,1.,0.)) ;
#11913 = DIRECTION('ref_axis',(-0.847998304005088,0.,-0.529998940003181)) ;
#11914 = DIRECTION('',(0.52999894000318,0.,-0.847998304005088)) ;
#11915 = DIRECTION('center_axis',(0.,1.,0.)) ;
#11916 = DIRECTION('ref_axis',(0.847998304005085,0.,0.529998940003185)) ;
#11917 = DIRECTION('center_axis',(0.,-1.,0.)) ;
#11918 = DIRECTION('ref_axis',(1.,0.,0.)) ;
#11919 = DIRECTION('center_axis',(-0.847998304005088,0.,-0.52999894000318)) ;
#11920 = DIRECTION('ref_axis',(-0.52999894000318,0.,0.847998304005088)) ;
#11921 = DIRECTION('',(-0.52999894000318,0.,0.847998304005088)) ;
#11922 = DIRECTION('',(0.,1.,0.)) ;
#11923 = DIRECTION('center_axis',(0.,1.,0.)) ;
#11924 = DIRECTION('ref_axis',(1.,0.,0.)) ;
#11925 = DIRECTION('',(0.,-1.,0.)) ;
#11926 = DIRECTION('center_axis',(0.,-1.,0.)) ;
#11927 = DIRECTION('ref_axis',(1.,0.,0.)) ;
#11928 = DIRECTION('center_axis',(0.,1.,0.)) ;
#11929 = DIRECTION('ref_axis',(0.847998304005085,0.,0.529998940003185)) ;
#11930 = DIRECTION('',(0.,1.,0.)) ;
#11931 = DIRECTION('center_axis',(0.,1.,0.)) ;
#11932 = DIRECTION('ref_axis',(0.847998304005085,0.,0.529998940003185)) ;
#11933 = DIRECTION('center_axis',(0.847998304005088,0.,0.52999894000318)) ;
#11934 = DIRECTION('ref_axis',(0.52999894000318,0.,-0.847998304005088)) ;
#11935 = DIRECTION('',(0.52999894000318,0.,-0.847998304005088)) ;
#11936 = DIRECTION('',(0.,1.,0.)) ;
#11937 = DIRECTION('center_axis',(0.,1.,0.)) ;
#11938 = DIRECTION('ref_axis',(-0.847998304005088,0.,-0.529998940003181)) ;
#11939 = DIRECTION('center_axis',(0.,1.,0.)) ;
#11940 = DIRECTION('ref_axis',(-0.847998304005088,0.,-0.529998940003181)) ;
#11941 = DIRECTION('center_axis',(0.,1.,0.)) ;
#11942 = DIRECTION('ref_axis',(1.,0.,0.)) ;
#11943 = DIRECTION('axis',(0.,0.,1.)) ;
#11944 = DIRECTION('refdir',(1.,0.,0.)) ;
#11945 = DIRECTION('center_axis',(-1.,0.,0.)) ;
#11946 = DIRECTION('ref_axis',(0.,0.,-1.)) ;
#11947 = DIRECTION('',(-1.,0.,0.)) ;
#11948 = DIRECTION('center_axis',(-1.,0.,0.)) ;
#11949 = DIRECTION('ref_axis',(0.,0.,-1.)) ;
#11950 = DIRECTION('',(-1.,0.,0.)) ;
#11951 = DIRECTION('center_axis',(0.,1.,0.)) ;
#11952 = DIRECTION('ref_axis',(1.,0.,0.)) ;
#11953 = DIRECTION('center_axis',(0.,1.,0.)) ;
#11954 = DIRECTION('ref_axis',(1.,0.,0.)) ;
#11955 = DIRECTION('',(0.,1.,0.)) ;
#11956 = DIRECTION('center_axis',(0.,-1.,0.)) ;
#11957 = DIRECTION('ref_axis',(1.,0.,0.)) ;
#11958 = DIRECTION('center_axis',(0.,0.,1.)) ;
#11959 = DIRECTION('ref_axis',(1.,0.,0.)) ;
#11960 = DIRECTION('center_axis',(0.,0.,1.)) ;
#11961 = DIRECTION('ref_axis',(1.,0.,0.)) ;
#11962 = DIRECTION('',(0.,-1.,0.)) ;
#11963 = DIRECTION('',(1.,0.,0.)) ;
#11964 = DIRECTION('',(0.,1.,0.)) ;
#11965 = DIRECTION('',(-1.,0.,0.)) ;
#11966 = DIRECTION('',(0.,-1.,0.)) ;
#11967 = DIRECTION('center_axis',(-1.,0.,0.)) ;
#11968 = DIRECTION('ref_axis',(0.,-1.,0.)) ;
#11969 = DIRECTION('',(0.,0.,1.)) ;
#11970 = DIRECTION('',(0.,-1.,0.)) ;
#11971 = DIRECTION('',(0.,0.,1.)) ;
#11972 = DIRECTION('center_axis',(0.,1.,0.)) ;
#11973 = DIRECTION('ref_axis',(-1.,0.,0.)) ;
#11974 = DIRECTION('',(-1.,0.,0.)) ;
#11975 = DIRECTION('',(0.,0.,1.)) ;
#11976 = DIRECTION('',(0.,0.,1.)) ;
#11977 = DIRECTION('center_axis',(1.,0.,0.)) ;
#11978 = DIRECTION('ref_axis',(0.,1.,0.)) ;
#11979 = DIRECTION('',(0.,1.,0.)) ;
#11980 = DIRECTION('',(0.,0.,1.)) ;
#11981 = DIRECTION('center_axis',(0.,-1.,0.)) ;
#11982 = DIRECTION('ref_axis',(1.,0.,0.)) ;
#11983 = DIRECTION('',(1.,0.,0.)) ;
#11984 = DIRECTION('center_axis',(-1.,0.,0.)) ;
#11985 = DIRECTION('ref_axis',(0.,-1.,0.)) ;
#11986 = DIRECTION('',(0.,0.,-1.)) ;
#11987 = DIRECTION('',(0.,-1.,0.)) ;
#11988 = DIRECTION('center_axis',(0.,0.,1.)) ;
#11989 = DIRECTION('ref_axis',(1.,0.,0.)) ;
#11990 = DIRECTION('center_axis',(0.,0.,-1.)) ;
#11991 = DIRECTION('ref_axis',(1.,0.,0.)) ;
#11992 = DIRECTION('center_axis',(0.,0.,-1.)) ;
#11993 = DIRECTION('ref_axis',(1.,0.,0.)) ;
#11994 = DIRECTION('center_axis',(0.,-3.67517835871524E-15,-1.)) ;
#11995 = DIRECTION('ref_axis',(1.,0.,0.)) ;
#11996 = DIRECTION('',(0.,0.,1.)) ;
#11997 = DIRECTION('',(0.,0.,1.)) ;
#11998 = DIRECTION('center_axis',(0.,-3.67517835871524E-15,-1.)) ;
#11999 = DIRECTION('ref_axis',(1.,0.,0.)) ;
#12000 = DIRECTION('center_axis',(0.,-3.67517835871524E-15,-1.)) ;
#12001 = DIRECTION('ref_axis',(1.,0.,0.)) ;
#12002 = DIRECTION('center_axis',(1.,0.,0.)) ;
#12003 = DIRECTION('ref_axis',(0.,0.,-1.)) ;
#12004 = DIRECTION('center_axis',(-1.,0.,0.)) ;
#12005 = DIRECTION('ref_axis',(0.,0.,-1.)) ;
#12006 = DIRECTION('center_axis',(0.,-1.,1.83758917935762E-15)) ;
#12007 = DIRECTION('ref_axis',(1.,0.,0.)) ;
#12008 = DIRECTION('center_axis',(0.,-1.,1.83758917935762E-15)) ;
#12009 = DIRECTION('ref_axis',(1.,0.,0.)) ;
#12010 = DIRECTION('center_axis',(0.,-1.,0.)) ;
#12011 = DIRECTION('ref_axis',(1.,0.,0.)) ;
#12012 = DIRECTION('',(0.,1.,0.)) ;
#12013 = DIRECTION('center_axis',(0.,-1.,1.83758917935762E-15)) ;
#12014 = DIRECTION('ref_axis',(1.,0.,0.)) ;
#12015 = DIRECTION('center_axis',(0.,-1.,1.83758917935762E-15)) ;
#12016 = DIRECTION('ref_axis',(1.,0.,0.)) ;
#12017 = DIRECTION('center_axis',(1.,0.,0.)) ;
#12018 = DIRECTION('ref_axis',(0.,0.,-1.)) ;
#12019 = DIRECTION('center_axis',(-1.,0.,0.)) ;
#12020 = DIRECTION('ref_axis',(0.,0.,-1.)) ;
#12021 = DIRECTION('center_axis',(0.,0.,1.)) ;
#12022 = DIRECTION('ref_axis',(1.,0.,0.)) ;
#12023 = DIRECTION('center_axis',(0.,0.,1.)) ;
#12024 = DIRECTION('ref_axis',(1.,0.,0.)) ;
#12025 = DIRECTION('center_axis',(0.,0.,1.)) ;
#12026 = DIRECTION('ref_axis',(1.,0.,0.)) ;
#12027 = DIRECTION('',(0.,0.,-1.)) ;
#12028 = DIRECTION('',(0.,0.,-1.)) ;
#12029 = DIRECTION('center_axis',(0.,0.,1.)) ;
#12030 = DIRECTION('ref_axis',(1.,0.,0.)) ;
#12031 = DIRECTION('center_axis',(0.,-3.67517835871524E-15,-1.)) ;
#12032 = DIRECTION('ref_axis',(1.,0.,0.)) ;
#12033 = DIRECTION('center_axis',(0.,0.,1.)) ;
#12034 = DIRECTION('ref_axis',(1.,0.,0.)) ;
#12035 = DIRECTION('axis',(0.,0.,1.)) ;
#12036 = DIRECTION('refdir',(1.,0.,0.)) ;
#12037 = DIRECTION('center_axis',(0.,1.,0.)) ;
#12038 = DIRECTION('ref_axis',(1.,0.,0.)) ;
#12039 = DIRECTION('center_axis',(0.,-1.,0.)) ;
#12040 = DIRECTION('ref_axis',(1.,0.,0.)) ;
#12041 = DIRECTION('',(0.,-1.,0.)) ;
#12042 = DIRECTION('center_axis',(0.,-1.,0.)) ;
#12043 = DIRECTION('ref_axis',(1.,0.,0.)) ;
#12044 = DIRECTION('center_axis',(0.985548890759753,0.,-0.169391215599333)) ;
#12045 = DIRECTION('ref_axis',(-0.169391215599333,0.,-0.985548890759753)) ;
#12046 = DIRECTION('',(-0.169391215599333,0.,-0.985548890759753)) ;
#12047 = DIRECTION('',(0.,1.,0.)) ;
#12048 = DIRECTION('',(-0.169391215599333,0.,-0.985548890759753)) ;
#12049 = DIRECTION('',(0.,1.,0.)) ;
#12050 = DIRECTION('center_axis',(0.,1.,0.)) ;
#12051 = DIRECTION('ref_axis',(-0.985548890759752,0.,0.169391215599339)) ;
#12052 = DIRECTION('center_axis',(0.,1.,0.)) ;
#12053 = DIRECTION('ref_axis',(-0.985548890759752,0.,0.169391215599339)) ;
#12054 = DIRECTION('center_axis',(0.,1.,0.)) ;
#12055 = DIRECTION('ref_axis',(-0.985548890759752,0.,0.169391215599339)) ;
#12056 = DIRECTION('',(0.,1.,0.)) ;
#12057 = DIRECTION('center_axis',(-0.985548890759753,0.,0.169391215599333)) ;
#12058 = DIRECTION('ref_axis',(0.169391215599333,0.,0.985548890759753)) ;
#12059 = DIRECTION('',(0.169391215599333,0.,0.985548890759753)) ;
#12060 = DIRECTION('',(0.169391215599333,0.,0.985548890759753)) ;
#12061 = DIRECTION('',(0.,1.,0.)) ;
#12062 = DIRECTION('center_axis',(0.,1.,0.)) ;
#12063 = DIRECTION('ref_axis',(0.985548890759754,0.,-0.16939121559933)) ;
#12064 = DIRECTION('center_axis',(0.,1.,0.)) ;
#12065 = DIRECTION('ref_axis',(0.985548890759754,0.,-0.16939121559933)) ;
#12066 = DIRECTION('center_axis',(0.,1.,0.)) ;
#12067 = DIRECTION('ref_axis',(0.985548890759754,0.,-0.16939121559933)) ;
#12068 = DIRECTION('center_axis',(0.,1.,0.)) ;
#12069 = DIRECTION('ref_axis',(1.,0.,0.)) ;
#12070 = DIRECTION('center_axis',(0.,1.,0.)) ;
#12071 = DIRECTION('ref_axis',(1.,0.,0.)) ;
#12072 = DIRECTION('axis',(0.,0.,1.)) ;
#12073 = DIRECTION('refdir',(1.,0.,0.)) ;
#12074 = DIRECTION('center_axis',(0.,1.,0.)) ;
#12075 = DIRECTION('ref_axis',(0.,0.,1.)) ;
#12076 = DIRECTION('center_axis',(0.,-1.,0.)) ;
#12077 = DIRECTION('ref_axis',(1.,0.,0.)) ;
#12078 = DIRECTION('center_axis',(0.,-1.,0.)) ;
#12079 = DIRECTION('ref_axis',(1.,0.,0.)) ;
#12080 = DIRECTION('center_axis',(0.,-1.,0.)) ;
#12081 = DIRECTION('ref_axis',(1.,0.,0.)) ;
#12082 = DIRECTION('',(0.707106781186563,0.707106781186532,8.65956056235513E-17)) ;
#12083 = DIRECTION('center_axis',(0.,-1.,0.)) ;
#12084 = DIRECTION('ref_axis',(1.,0.,0.)) ;
#12085 = DIRECTION('center_axis',(0.,-1.,0.)) ;
#12086 = DIRECTION('ref_axis',(1.,0.,0.)) ;
#12087 = DIRECTION('',(0.,1.,0.)) ;
#12088 = DIRECTION('center_axis',(0.,-1.,0.)) ;
#12089 = DIRECTION('ref_axis',(0.,0.,-1.)) ;
#12090 = DIRECTION('center_axis',(0.,-1.,0.)) ;
#12091 = DIRECTION('ref_axis',(1.,0.,0.)) ;
#12092 = DIRECTION('center_axis',(0.,-1.,0.)) ;
#12093 = DIRECTION('ref_axis',(1.,0.,0.)) ;
#12094 = DIRECTION('center_axis',(0.,-1.,0.)) ;
#12095 = DIRECTION('ref_axis',(1.,0.,0.)) ;
#12096 = DIRECTION('',(0.,1.,0.)) ;
#12097 = DIRECTION('center_axis',(0.,-1.,0.)) ;
#12098 = DIRECTION('ref_axis',(0.,0.,-1.)) ;
#12099 = DIRECTION('center_axis',(0.,-1.,0.)) ;
#12100 = DIRECTION('ref_axis',(1.,0.,0.)) ;
#12101 = DIRECTION('center_axis',(0.,-1.,0.)) ;
#12102 = DIRECTION('ref_axis',(1.,0.,0.)) ;
#12103 = DIRECTION('center_axis',(0.,-1.,0.)) ;
#12104 = DIRECTION('ref_axis',(1.,0.,0.)) ;
#12105 = DIRECTION('',(0.,1.,0.)) ;
#12106 = DIRECTION('center_axis',(0.,1.,0.)) ;
#12107 = DIRECTION('ref_axis',(0.,0.,1.)) ;
#12108 = DIRECTION('center_axis',(0.,-1.,0.)) ;
#12109 = DIRECTION('ref_axis',(1.,0.,0.)) ;
#12110 = DIRECTION('center_axis',(0.,-1.,0.)) ;
#12111 = DIRECTION('ref_axis',(1.,0.,0.)) ;
#12112 = DIRECTION('center_axis',(0.,-1.,0.)) ;
#12113 = DIRECTION('ref_axis',(1.,0.,0.)) ;
#12114 = DIRECTION('',(0.,1.,0.)) ;
#12115 = DIRECTION('center_axis',(0.,1.,0.)) ;
#12116 = DIRECTION('ref_axis',(1.,0.,0.)) ;
#12117 = DIRECTION('center_axis',(0.,-1.,0.)) ;
#12118 = DIRECTION('ref_axis',(1.,0.,0.)) ;
#12119 = DIRECTION('',(-0.707106781186548,0.707106781186547,-8.65956056235493E-17)) ;
#12120 = DIRECTION('center_axis',(0.,-1.,0.)) ;
#12121 = DIRECTION('ref_axis',(0.,0.,-1.)) ;
#12122 = DIRECTION('axis',(0.,0.,1.)) ;
#12123 = DIRECTION('refdir',(1.,0.,0.)) ;
#12124 = DIRECTION('center_axis',(0.,0.,1.)) ;
#12125 = DIRECTION('ref_axis',(1.,0.,0.)) ;
#12126 = DIRECTION('',(1.,0.,0.)) ;
#12127 = DIRECTION('',(0.,-1.,0.)) ;
#12128 = DIRECTION('',(-1.,0.,0.)) ;
#12129 = DIRECTION('',(0.,1.,0.)) ;
#12130 = DIRECTION('center_axis',(0.,0.,1.)) ;
#12131 = DIRECTION('ref_axis',(1.,0.,0.)) ;
#12132 = DIRECTION('',(1.,0.,0.)) ;
#12133 = DIRECTION('',(0.,1.,0.)) ;
#12134 = DIRECTION('',(-1.,0.,0.)) ;
#12135 = DIRECTION('',(0.,1.,0.)) ;
#12136 = DIRECTION('center_axis',(1.,0.,0.)) ;
#12137 = DIRECTION('ref_axis',(0.,0.,-1.)) ;
#12138 = DIRECTION('',(0.,0.,-1.)) ;
#12139 = DIRECTION('',(0.,0.,1.)) ;
#12140 = DIRECTION('',(0.,1.,0.)) ;
#12141 = DIRECTION('center_axis',(-1.,0.,0.)) ;
#12142 = DIRECTION('ref_axis',(0.,0.,1.)) ;
#12143 = DIRECTION('',(0.,0.,1.)) ;
#12144 = DIRECTION('',(0.,-1.,0.)) ;
#12145 = DIRECTION('',(0.,0.,-1.)) ;
#12146 = DIRECTION('center_axis',(0.,-1.,0.)) ;
#12147 = DIRECTION('ref_axis',(-1.83697019872103E-16,0.,1.)) ;
#12148 = DIRECTION('center_axis',(0.,-1.,0.)) ;
#12149 = DIRECTION('ref_axis',(1.,0.,0.)) ;
#12150 = DIRECTION('center_axis',(0.,-1.,0.)) ;
#12151 = DIRECTION('ref_axis',(1.,0.,0.)) ;
#12152 = DIRECTION('center_axis',(0.,1.,0.)) ;
#12153 = DIRECTION('ref_axis',(0.,0.,1.)) ;
#12154 = DIRECTION('center_axis',(0.,-1.,0.)) ;
#12155 = DIRECTION('ref_axis',(1.,0.,0.)) ;
#12156 = DIRECTION('center_axis',(0.,-1.,0.)) ;
#12157 = DIRECTION('ref_axis',(-1.83697019872103E-16,0.,1.)) ;
#12158 = DIRECTION('center_axis',(0.,-1.,0.)) ;
#12159 = DIRECTION('ref_axis',(1.,0.,0.)) ;
#12160 = DIRECTION('center_axis',(0.,-1.,0.)) ;
#12161 = DIRECTION('ref_axis',(0.,0.,-1.)) ;
#12162 = DIRECTION('axis',(0.,0.,1.)) ;
#12163 = DIRECTION('refdir',(1.,0.,0.)) ;
#12164 = DIRECTION('center_axis',(0.,1.,0.)) ;
#12165 = DIRECTION('ref_axis',(0.,0.,1.)) ;
#12166 = DIRECTION('center_axis',(0.,-1.,0.)) ;
#12167 = DIRECTION('ref_axis',(1.,0.,0.)) ;
#12168 = DIRECTION('center_axis',(0.,-1.,0.)) ;
#12169 = DIRECTION('ref_axis',(1.,0.,0.)) ;
#12170 = DIRECTION('center_axis',(0.,-1.,0.)) ;
#12171 = DIRECTION('ref_axis',(1.,0.,0.)) ;
#12172 = DIRECTION('',(0.707106781186537,0.707106781186558,8.6595605623548E-17)) ;
#12173 = DIRECTION('center_axis',(0.,-1.,0.)) ;
#12174 = DIRECTION('ref_axis',(1.,0.,0.)) ;
#12175 = DIRECTION('center_axis',(0.,-1.,0.)) ;
#12176 = DIRECTION('ref_axis',(1.,0.,0.)) ;
#12177 = DIRECTION('',(0.,1.,0.)) ;
#12178 = DIRECTION('center_axis',(0.,1.,0.)) ;
#12179 = DIRECTION('ref_axis',(1.,0.,0.)) ;
#12180 = DIRECTION('center_axis',(0.,-1.,0.)) ;
#12181 = DIRECTION('ref_axis',(1.,0.,0.)) ;
#12182 = DIRECTION('',(-0.707106781186547,0.707106781186547,-8.65956056235493E-17)) ;
#12183 = DIRECTION('center_axis',(0.,-1.,0.)) ;
#12184 = DIRECTION('ref_axis',(0.,0.,-1.)) ;
#12185 = DIRECTION('center_axis',(0.,-1.,0.)) ;
#12186 = DIRECTION('ref_axis',(1.,0.,0.)) ;
#12187 = DIRECTION('center_axis',(0.,-1.,0.)) ;
#12188 = DIRECTION('ref_axis',(1.,0.,0.)) ;
#12189 = DIRECTION('center_axis',(0.,-1.,0.)) ;
#12190 = DIRECTION('ref_axis',(1.,0.,0.)) ;
#12191 = DIRECTION('',(0.,1.,0.)) ;
#12192 = DIRECTION('center_axis',(0.,1.,0.)) ;
#12193 = DIRECTION('ref_axis',(1.,0.,0.)) ;
#12194 = DIRECTION('center_axis',(0.,-1.,0.)) ;
#12195 = DIRECTION('ref_axis',(1.,0.,0.)) ;
#12196 = DIRECTION('',(-0.707106781186548,0.707106781186548,-8.65956056235493E-17)) ;
#12197 = DIRECTION('center_axis',(0.,-1.,0.)) ;
#12198 = DIRECTION('ref_axis',(0.,0.,-1.)) ;
#12199 = DIRECTION('axis',(0.,0.,1.)) ;
#12200 = DIRECTION('refdir',(1.,0.,0.)) ;
#12201 = DIRECTION('center_axis',(0.,0.,1.)) ;
#12202 = DIRECTION('ref_axis',(1.,0.,0.)) ;
#12203 = DIRECTION('',(0.,0.,-1.)) ;
#12204 = DIRECTION('center_axis',(0.,0.,-1.)) ;
#12205 = DIRECTION('ref_axis',(1.,0.,0.)) ;
#12206 = DIRECTION('center_axis',(0.,0.,1.)) ;
#12207 = DIRECTION('ref_axis',(1.,0.,0.)) ;
#12208 = DIRECTION('',(0.,0.,-1.)) ;
#12209 = DIRECTION('center_axis',(0.,0.,1.)) ;
#12210 = DIRECTION('ref_axis',(1.,0.,0.)) ;
#12211 = DIRECTION('',(0.,0.,-1.)) ;
#12212 = DIRECTION('center_axis',(0.,0.,1.)) ;
#12213 = DIRECTION('ref_axis',(1.,0.,0.)) ;
#12214 = DIRECTION('',(0.,0.,-1.)) ;
#12215 = DIRECTION('center_axis',(0.,0.,1.)) ;
#12216 = DIRECTION('ref_axis',(1.,0.,0.)) ;
#12217 = DIRECTION('',(0.,0.,-1.)) ;
#12218 = DIRECTION('center_axis',(0.,0.,1.)) ;
#12219 = DIRECTION('ref_axis',(1.,0.,0.)) ;
#12220 = DIRECTION('',(0.,0.,-1.)) ;
#12221 = DIRECTION('center_axis',(0.,0.,1.)) ;
#12222 = DIRECTION('ref_axis',(1.,0.,0.)) ;
#12223 = DIRECTION('',(0.,0.,-1.)) ;
#12224 = DIRECTION('center_axis',(0.,0.,1.)) ;
#12225 = DIRECTION('ref_axis',(1.,0.,0.)) ;
#12226 = DIRECTION('',(0.,0.,-1.)) ;
#12227 = DIRECTION('center_axis',(0.,0.,1.)) ;
#12228 = DIRECTION('ref_axis',(1.,0.,0.)) ;
#12229 = DIRECTION('',(0.,0.,-1.)) ;
#12230 = DIRECTION('center_axis',(0.,0.,1.)) ;
#12231 = DIRECTION('ref_axis',(1.,0.,0.)) ;
#12232 = DIRECTION('',(0.,0.,-1.)) ;
#12233 = DIRECTION('center_axis',(0.,0.,1.)) ;
#12234 = DIRECTION('ref_axis',(1.,0.,0.)) ;
#12235 = DIRECTION('',(0.,0.,-1.)) ;
#12236 = DIRECTION('center_axis',(0.,0.,1.)) ;
#12237 = DIRECTION('ref_axis',(1.,0.,0.)) ;
#12238 = DIRECTION('',(0.,0.,-1.)) ;
#12239 = DIRECTION('center_axis',(0.,0.,1.)) ;
#12240 = DIRECTION('ref_axis',(1.,0.,0.)) ;
#12241 = DIRECTION('',(0.,0.,-1.)) ;
#12242 = DIRECTION('center_axis',(0.,0.,1.)) ;
#12243 = DIRECTION('ref_axis',(1.,0.,0.)) ;
#12244 = DIRECTION('',(0.,0.,-1.)) ;
#12245 = DIRECTION('center_axis',(0.,0.,1.)) ;
#12246 = DIRECTION('ref_axis',(-0.762712670465396,-0.646737491036004,0.)) ;
#12247 = DIRECTION('',(0.,0.,1.)) ;
#12248 = DIRECTION('center_axis',(0.,0.,1.)) ;
#12249 = DIRECTION('ref_axis',(1.,1.08167872493926E-13,0.)) ;
#12250 = DIRECTION('center_axis',(0.,0.,1.)) ;
#12251 = DIRECTION('ref_axis',(1.,1.08167872493926E-13,0.)) ;
#12252 = DIRECTION('',(0.,0.,1.)) ;
#12253 = DIRECTION('center_axis',(0.,0.,1.)) ;
#12254 = DIRECTION('ref_axis',(1.,1.08167872493926E-13,0.)) ;
#12255 = DIRECTION('',(0.,0.,1.)) ;
#12256 = DIRECTION('center_axis',(0.,0.,1.)) ;
#12257 = DIRECTION('ref_axis',(1.,1.08167872493926E-13,0.)) ;
#12258 = DIRECTION('',(0.,0.,1.)) ;
#12259 = DIRECTION('center_axis',(0.,0.,1.)) ;
#12260 = DIRECTION('ref_axis',(1.,1.08167872493926E-13,0.)) ;
#12261 = DIRECTION('',(0.,0.,1.)) ;
#12262 = DIRECTION('center_axis',(0.,0.,1.)) ;
#12263 = DIRECTION('ref_axis',(1.,1.08167872493926E-13,0.)) ;
#12264 = DIRECTION('',(0.,0.,1.)) ;
#12265 = DIRECTION('center_axis',(0.,0.,1.)) ;
#12266 = DIRECTION('ref_axis',(1.,1.08167872493926E-13,0.)) ;
#12267 = DIRECTION('',(0.,0.,1.)) ;
#12268 = DIRECTION('center_axis',(0.,0.,1.)) ;
#12269 = DIRECTION('ref_axis',(1.,1.08167872493926E-13,0.)) ;
#12270 = DIRECTION('',(0.,0.,1.)) ;
#12271 = DIRECTION('center_axis',(0.,0.,1.)) ;
#12272 = DIRECTION('ref_axis',(1.,1.08167872493926E-13,0.)) ;
#12273 = DIRECTION('',(0.,0.,1.)) ;
#12274 = DIRECTION('center_axis',(0.,0.,1.)) ;
#12275 = DIRECTION('ref_axis',(1.,1.08167872493926E-13,0.)) ;
#12276 = DIRECTION('',(0.,0.,1.)) ;
#12277 = DIRECTION('center_axis',(0.,0.,1.)) ;
#12278 = DIRECTION('ref_axis',(1.,1.08167872493926E-13,0.)) ;
#12279 = DIRECTION('',(0.,0.,1.)) ;
#12280 = DIRECTION('center_axis',(0.,0.,1.)) ;
#12281 = DIRECTION('ref_axis',(1.,1.08167872493926E-13,0.)) ;
#12282 = DIRECTION('',(0.,0.,1.)) ;
#12283 = DIRECTION('center_axis',(0.,0.,1.)) ;
#12284 = DIRECTION('ref_axis',(1.,1.08167872493926E-13,0.)) ;
#12285 = DIRECTION('',(0.,0.,1.)) ;
#12286 = DIRECTION('center_axis',(0.,0.,1.)) ;
#12287 = DIRECTION('ref_axis',(1.,1.08167872493926E-13,0.)) ;
#12288 = DIRECTION('',(0.,0.,1.)) ;
#12289 = DIRECTION('center_axis',(0.,0.,1.)) ;
#12290 = DIRECTION('ref_axis',(1.,0.,0.)) ;
#12291 = DIRECTION('center_axis',(0.,0.,1.)) ;
#12292 = DIRECTION('ref_axis',(1.,0.,0.)) ;
#12293 = DIRECTION('center_axis',(0.,0.,1.)) ;
#12294 = DIRECTION('ref_axis',(1.,0.,0.)) ;
#12295 = DIRECTION('center_axis',(0.,0.,1.)) ;
#12296 = DIRECTION('ref_axis',(1.,0.,0.)) ;
#12297 = DIRECTION('center_axis',(0.,0.,-1.)) ;
#12298 = DIRECTION('ref_axis',(1.,0.,0.)) ;
#12299 = DIRECTION('center_axis',(0.,0.,-1.)) ;
#12300 = DIRECTION('ref_axis',(1.,1.08167872493926E-13,0.)) ;
#12301 = DIRECTION('center_axis',(0.,0.,-1.)) ;
#12302 = DIRECTION('ref_axis',(1.,0.,0.)) ;
#12303 = DIRECTION('center_axis',(0.,0.,1.)) ;
#12304 = DIRECTION('ref_axis',(1.,1.08167872493926E-13,0.)) ;
#12305 = DIRECTION('center_axis',(0.,0.,-1.)) ;
#12306 = DIRECTION('ref_axis',(-1.,0.,0.)) ;
#12307 = DIRECTION('center_axis',(0.,-1.,0.)) ;
#12308 = DIRECTION('ref_axis',(1.,0.,0.)) ;
#12309 = DIRECTION('center_axis',(0.,0.,1.)) ;
#12310 = DIRECTION('ref_axis',(1.,0.,0.)) ;
#12311 = DIRECTION('center_axis',(0.,0.,1.)) ;
#12312 = DIRECTION('ref_axis',(0.581478264894299,-0.813561938303111,0.)) ;
#12313 = DIRECTION('center_axis',(0.,0.,1.)) ;
#12314 = DIRECTION('ref_axis',(1.,0.,0.)) ;
#12315 = DIRECTION('center_axis',(0.,0.,1.)) ;
#12316 = DIRECTION('ref_axis',(1.,0.,0.)) ;
#12317 = DIRECTION('center_axis',(0.,0.,-1.)) ;
#12318 = DIRECTION('ref_axis',(1.,0.,0.)) ;
#12319 = DIRECTION('center_axis',(0.,0.,-1.)) ;
#12320 = DIRECTION('ref_axis',(1.,0.,0.)) ;
#12321 = DIRECTION('',(0.707106781186547,-8.65956056235493E-17,0.707106781186547)) ;
#12322 = DIRECTION('center_axis',(0.,0.,-1.)) ;
#12323 = DIRECTION('ref_axis',(1.,0.,0.)) ;
#12324 = DIRECTION('center_axis',(0.,0.,1.)) ;
#12325 = DIRECTION('ref_axis',(1.,0.,0.)) ;
#12326 = DIRECTION('center_axis',(0.,0.,1.)) ;
#12327 = DIRECTION('ref_axis',(0.984807753012208,-0.17364817766693,0.)) ;
#12328 = DIRECTION('center_axis',(0.,0.,1.)) ;
#12329 = DIRECTION('ref_axis',(1.,0.,0.)) ;
#12330 = DIRECTION('',(0.869726513699841,-0.493533981978465,0.)) ;
#12331 = DIRECTION('',(-0.986074150277955,-0.166306254102512,0.)) ;
#12332 = DIRECTION('center_axis',(-0.166306254102512,0.986074150277955,0.)) ;
#12333 = DIRECTION('ref_axis',(-0.986074150277955,-0.166306254102512,0.)) ;
#12334 = DIRECTION('',(0.,0.,-1.)) ;
#12335 = DIRECTION('',(0.,0.,1.)) ;
#12336 = DIRECTION('center_axis',(-0.493533981978465,-0.869726513699841,0.)) ;
#12337 = DIRECTION('ref_axis',(0.869726513699841,-0.493533981978465,0.)) ;
#12338 = DIRECTION('',(0.,0.,1.)) ;
#12339 = DIRECTION('center_axis',(0.,0.,-1.)) ;
#12340 = DIRECTION('ref_axis',(1.,0.,0.)) ;
#12341 = DIRECTION('center_axis',(0.,0.,-1.)) ;
#12342 = DIRECTION('ref_axis',(1.,0.,0.)) ;
#12343 = DIRECTION('',(0.,0.,1.)) ;
#12344 = DIRECTION('center_axis',(0.,0.,1.)) ;
#12345 = DIRECTION('ref_axis',(1.,0.,0.)) ;
#12346 = DIRECTION('',(0.,0.,-1.)) ;
#12347 = DIRECTION('center_axis',(0.,0.,-1.)) ;
#12348 = DIRECTION('ref_axis',(1.,0.,0.)) ;
#12349 = DIRECTION('',(0.,0.,1.)) ;
#12350 = DIRECTION('center_axis',(0.,0.,1.)) ;
#12351 = DIRECTION('ref_axis',(1.,0.,0.)) ;
#12352 = DIRECTION('',(0.,0.,-1.)) ;
#12353 = DIRECTION('center_axis',(0.,0.,-1.)) ;
#12354 = DIRECTION('ref_axis',(1.,0.,0.)) ;
#12355 = DIRECTION('',(0.,0.,1.)) ;
#12356 = DIRECTION('center_axis',(0.,0.,1.)) ;
#12357 = DIRECTION('ref_axis',(1.,0.,0.)) ;
#12358 = DIRECTION('',(0.,0.,-1.)) ;
#12359 = DIRECTION('center_axis',(0.,0.,-1.)) ;
#12360 = DIRECTION('ref_axis',(1.,0.,0.)) ;
#12361 = DIRECTION('',(0.,0.,1.)) ;
#12362 = DIRECTION('center_axis',(0.,0.,1.)) ;
#12363 = DIRECTION('ref_axis',(1.,0.,0.)) ;
#12364 = DIRECTION('',(0.,0.,-1.)) ;
#12365 = DIRECTION('center_axis',(0.,0.,-1.)) ;
#12366 = DIRECTION('ref_axis',(1.,0.,0.)) ;
#12367 = DIRECTION('',(0.,0.,1.)) ;
#12368 = DIRECTION('center_axis',(0.,0.,1.)) ;
#12369 = DIRECTION('ref_axis',(1.,0.,0.)) ;
#12370 = DIRECTION('',(0.,0.,-1.)) ;
#12371 = DIRECTION('center_axis',(0.,0.,-1.)) ;
#12372 = DIRECTION('ref_axis',(1.,0.,0.)) ;
#12373 = DIRECTION('',(0.,0.,1.)) ;
#12374 = DIRECTION('center_axis',(0.,0.,1.)) ;
#12375 = DIRECTION('ref_axis',(1.,0.,0.)) ;
#12376 = DIRECTION('',(0.,0.,-1.)) ;
#12377 = DIRECTION('center_axis',(0.,0.,-1.)) ;
#12378 = DIRECTION('ref_axis',(1.,0.,0.)) ;
#12379 = DIRECTION('',(0.,0.,1.)) ;
#12380 = DIRECTION('center_axis',(0.,0.,1.)) ;
#12381 = DIRECTION('ref_axis',(1.,0.,0.)) ;
#12382 = DIRECTION('',(0.,0.,-1.)) ;
#12383 = DIRECTION('center_axis',(0.,0.,-1.)) ;
#12384 = DIRECTION('ref_axis',(1.,0.,0.)) ;
#12385 = DIRECTION('',(0.,0.,1.)) ;
#12386 = DIRECTION('center_axis',(0.,0.,1.)) ;
#12387 = DIRECTION('ref_axis',(1.,0.,0.)) ;
#12388 = DIRECTION('',(0.,0.,-1.)) ;
#12389 = DIRECTION('center_axis',(0.,0.,-1.)) ;
#12390 = DIRECTION('ref_axis',(1.,0.,0.)) ;
#12391 = DIRECTION('',(0.,0.,1.)) ;
#12392 = DIRECTION('center_axis',(0.,0.,1.)) ;
#12393 = DIRECTION('ref_axis',(1.,0.,0.)) ;
#12394 = DIRECTION('',(0.,0.,-1.)) ;
#12395 = DIRECTION('center_axis',(0.,0.,-1.)) ;
#12396 = DIRECTION('ref_axis',(1.,0.,0.)) ;
#12397 = DIRECTION('',(0.,0.,1.)) ;
#12398 = DIRECTION('center_axis',(0.,0.,1.)) ;
#12399 = DIRECTION('ref_axis',(1.,0.,0.)) ;
#12400 = DIRECTION('',(0.,0.,-1.)) ;
#12401 = DIRECTION('center_axis',(0.,0.,-1.)) ;
#12402 = DIRECTION('ref_axis',(1.,0.,0.)) ;
#12403 = DIRECTION('',(0.,0.,1.)) ;
#12404 = DIRECTION('center_axis',(0.,0.,1.)) ;
#12405 = DIRECTION('ref_axis',(1.,0.,0.)) ;
#12406 = DIRECTION('',(0.,0.,-1.)) ;
#12407 = DIRECTION('center_axis',(0.,0.,-1.)) ;
#12408 = DIRECTION('ref_axis',(1.,0.,0.)) ;
#12409 = DIRECTION('',(0.,0.,1.)) ;
#12410 = DIRECTION('center_axis',(0.,0.,1.)) ;
#12411 = DIRECTION('ref_axis',(1.,0.,0.)) ;
#12412 = DIRECTION('',(0.,0.,-1.)) ;
#12413 = DIRECTION('center_axis',(0.,0.,-1.)) ;
#12414 = DIRECTION('ref_axis',(1.,0.,0.)) ;
#12415 = DIRECTION('',(0.,0.,1.)) ;
#12416 = DIRECTION('center_axis',(0.,0.,1.)) ;
#12417 = DIRECTION('ref_axis',(1.,0.,0.)) ;
#12418 = DIRECTION('',(0.,0.,-1.)) ;
#12419 = DIRECTION('center_axis',(0.,0.,-1.)) ;
#12420 = DIRECTION('ref_axis',(1.,0.,0.)) ;
#12421 = DIRECTION('',(0.,0.,1.)) ;
#12422 = DIRECTION('center_axis',(0.,0.,1.)) ;
#12423 = DIRECTION('ref_axis',(1.,0.,0.)) ;
#12424 = DIRECTION('',(0.,0.,-1.)) ;
#12425 = DIRECTION('center_axis',(0.,0.,-1.)) ;
#12426 = DIRECTION('ref_axis',(1.,0.,0.)) ;
#12427 = DIRECTION('',(0.,0.,1.)) ;
#12428 = DIRECTION('center_axis',(0.,0.,1.)) ;
#12429 = DIRECTION('ref_axis',(1.,0.,0.)) ;
#12430 = DIRECTION('',(0.,0.,-1.)) ;
#12431 = DIRECTION('center_axis',(0.,0.,-1.)) ;
#12432 = DIRECTION('ref_axis',(1.,0.,0.)) ;
#12433 = DIRECTION('',(0.,0.,1.)) ;
#12434 = DIRECTION('center_axis',(0.,0.,1.)) ;
#12435 = DIRECTION('ref_axis',(1.,0.,0.)) ;
#12436 = DIRECTION('',(0.,0.,-1.)) ;
#12437 = DIRECTION('center_axis',(0.,0.,-1.)) ;
#12438 = DIRECTION('ref_axis',(1.,0.,0.)) ;
#12439 = DIRECTION('',(0.,0.,1.)) ;
#12440 = DIRECTION('center_axis',(0.,0.,1.)) ;
#12441 = DIRECTION('ref_axis',(1.,0.,0.)) ;
#12442 = DIRECTION('',(0.,0.,-1.)) ;
#12443 = DIRECTION('center_axis',(0.,0.,-1.)) ;
#12444 = DIRECTION('ref_axis',(1.,0.,0.)) ;
#12445 = DIRECTION('',(0.,0.,1.)) ;
#12446 = DIRECTION('center_axis',(0.,0.,1.)) ;
#12447 = DIRECTION('ref_axis',(1.,0.,0.)) ;
#12448 = DIRECTION('',(0.,0.,-1.)) ;
#12449 = DIRECTION('center_axis',(0.,0.,-1.)) ;
#12450 = DIRECTION('ref_axis',(1.,0.,0.)) ;
#12451 = DIRECTION('',(0.,0.,1.)) ;
#12452 = DIRECTION('center_axis',(0.,0.,1.)) ;
#12453 = DIRECTION('ref_axis',(1.,0.,0.)) ;
#12454 = DIRECTION('',(0.,0.,1.)) ;
#12455 = DIRECTION('center_axis',(0.,0.,1.)) ;
#12456 = DIRECTION('ref_axis',(1.,0.,0.)) ;
#12457 = DIRECTION('center_axis',(0.,0.,1.)) ;
#12458 = DIRECTION('ref_axis',(1.,0.,0.)) ;
#12459 = DIRECTION('',(0.,0.,-1.)) ;
#12460 = DIRECTION('center_axis',(0.,0.,-1.)) ;
#12461 = DIRECTION('ref_axis',(1.,0.,0.)) ;
#12462 = DIRECTION('',(0.,0.,1.)) ;
#12463 = DIRECTION('center_axis',(0.,0.,1.)) ;
#12464 = DIRECTION('ref_axis',(1.,0.,0.)) ;
#12465 = DIRECTION('',(0.,0.,-1.)) ;
#12466 = DIRECTION('center_axis',(0.,0.,-1.)) ;
#12467 = DIRECTION('ref_axis',(1.,0.,0.)) ;
#12468 = DIRECTION('',(0.,0.,1.)) ;
#12469 = DIRECTION('center_axis',(0.,0.,1.)) ;
#12470 = DIRECTION('ref_axis',(1.,0.,0.)) ;
#12471 = DIRECTION('',(0.,0.,-1.)) ;
#12472 = DIRECTION('center_axis',(0.,0.,-1.)) ;
#12473 = DIRECTION('ref_axis',(1.,0.,0.)) ;
#12474 = DIRECTION('',(0.,0.,1.)) ;
#12475 = DIRECTION('center_axis',(0.,0.,1.)) ;
#12476 = DIRECTION('ref_axis',(1.,0.,0.)) ;
#12477 = DIRECTION('',(0.,0.,-1.)) ;
#12478 = DIRECTION('center_axis',(0.,0.,-1.)) ;
#12479 = DIRECTION('ref_axis',(1.,0.,0.)) ;
#12480 = DIRECTION('',(0.,0.,1.)) ;
#12481 = DIRECTION('center_axis',(0.,0.,1.)) ;
#12482 = DIRECTION('ref_axis',(1.,0.,0.)) ;
#12483 = DIRECTION('',(0.,0.,-1.)) ;
#12484 = DIRECTION('center_axis',(0.,0.,-1.)) ;
#12485 = DIRECTION('ref_axis',(1.,0.,0.)) ;
#12486 = DIRECTION('',(0.,0.,1.)) ;
#12487 = DIRECTION('center_axis',(0.,0.,1.)) ;
#12488 = DIRECTION('ref_axis',(1.,0.,0.)) ;
#12489 = DIRECTION('',(0.,0.,-1.)) ;
#12490 = DIRECTION('center_axis',(0.,0.,-1.)) ;
#12491 = DIRECTION('ref_axis',(1.,0.,0.)) ;
#12492 = DIRECTION('',(0.,0.,1.)) ;
#12493 = DIRECTION('center_axis',(0.,0.,1.)) ;
#12494 = DIRECTION('ref_axis',(1.,0.,0.)) ;
#12495 = DIRECTION('',(0.,0.,-1.)) ;
#12496 = DIRECTION('center_axis',(0.,0.,-1.)) ;
#12497 = DIRECTION('ref_axis',(1.,0.,0.)) ;
#12498 = DIRECTION('',(0.,0.,1.)) ;
#12499 = DIRECTION('center_axis',(0.,0.,1.)) ;
#12500 = DIRECTION('ref_axis',(1.,0.,0.)) ;
#12501 = DIRECTION('',(0.,0.,-1.)) ;
#12502 = DIRECTION('center_axis',(0.,0.,-1.)) ;
#12503 = DIRECTION('ref_axis',(1.,0.,0.)) ;
#12504 = DIRECTION('',(0.,0.,1.)) ;
#12505 = DIRECTION('center_axis',(0.,0.,1.)) ;
#12506 = DIRECTION('ref_axis',(1.,0.,0.)) ;
#12507 = DIRECTION('',(0.,0.,-1.)) ;
#12508 = DIRECTION('center_axis',(0.,0.,-1.)) ;
#12509 = DIRECTION('ref_axis',(1.,0.,0.)) ;
#12510 = DIRECTION('',(0.,0.,1.)) ;
#12511 = DIRECTION('center_axis',(0.,0.,1.)) ;
#12512 = DIRECTION('ref_axis',(1.,0.,0.)) ;
#12513 = DIRECTION('',(0.,0.,-1.)) ;
#12514 = DIRECTION('center_axis',(0.,0.,-1.)) ;
#12515 = DIRECTION('ref_axis',(1.,0.,0.)) ;
#12516 = DIRECTION('',(0.,0.,1.)) ;
#12517 = DIRECTION('center_axis',(0.,0.,1.)) ;
#12518 = DIRECTION('ref_axis',(1.,0.,0.)) ;
#12519 = DIRECTION('',(0.,0.,-1.)) ;
#12520 = DIRECTION('center_axis',(0.,0.,-1.)) ;
#12521 = DIRECTION('ref_axis',(1.,0.,0.)) ;
#12522 = DIRECTION('',(0.,0.,1.)) ;
#12523 = DIRECTION('center_axis',(0.,0.,1.)) ;
#12524 = DIRECTION('ref_axis',(1.,0.,0.)) ;
#12525 = DIRECTION('',(0.,0.,-1.)) ;
#12526 = DIRECTION('center_axis',(0.,0.,-1.)) ;
#12527 = DIRECTION('ref_axis',(1.,0.,0.)) ;
#12528 = DIRECTION('',(0.,0.,1.)) ;
#12529 = DIRECTION('center_axis',(0.,0.,1.)) ;
#12530 = DIRECTION('ref_axis',(1.,0.,0.)) ;
#12531 = DIRECTION('',(0.,0.,-1.)) ;
#12532 = DIRECTION('center_axis',(0.,0.,-1.)) ;
#12533 = DIRECTION('ref_axis',(1.,0.,0.)) ;
#12534 = DIRECTION('',(0.,0.,1.)) ;
#12535 = DIRECTION('center_axis',(0.,0.,1.)) ;
#12536 = DIRECTION('ref_axis',(1.,0.,0.)) ;
#12537 = DIRECTION('',(0.,0.,-1.)) ;
#12538 = DIRECTION('center_axis',(0.,0.,-1.)) ;
#12539 = DIRECTION('ref_axis',(1.,0.,0.)) ;
#12540 = DIRECTION('',(0.,0.,1.)) ;
#12541 = DIRECTION('center_axis',(0.,0.,1.)) ;
#12542 = DIRECTION('ref_axis',(1.,0.,0.)) ;
#12543 = DIRECTION('',(0.,0.,-1.)) ;
#12544 = DIRECTION('center_axis',(0.,0.,-1.)) ;
#12545 = DIRECTION('ref_axis',(1.,0.,0.)) ;
#12546 = DIRECTION('',(0.,0.,1.)) ;
#12547 = DIRECTION('center_axis',(0.,0.,1.)) ;
#12548 = DIRECTION('ref_axis',(1.,0.,0.)) ;
#12549 = DIRECTION('',(0.,0.,-1.)) ;
#12550 = DIRECTION('center_axis',(0.,0.,-1.)) ;
#12551 = DIRECTION('ref_axis',(1.,0.,0.)) ;
#12552 = DIRECTION('',(0.,0.,1.)) ;
#12553 = DIRECTION('center_axis',(0.,0.,1.)) ;
#12554 = DIRECTION('ref_axis',(1.,0.,0.)) ;
#12555 = DIRECTION('',(0.,0.,-1.)) ;
#12556 = DIRECTION('center_axis',(0.,0.,-1.)) ;
#12557 = DIRECTION('ref_axis',(1.,0.,0.)) ;
#12558 = DIRECTION('center_axis',(0.0074502908256619,0.99997224619817,0.)) ;
#12559 = DIRECTION('ref_axis',(-0.99997224619817,0.0074502908256619,0.)) ;
#12560 = DIRECTION('',(-0.99997224619817,0.0074502908256619,0.)) ;
#12561 = DIRECTION('',(0.,0.,1.)) ;
#12562 = DIRECTION('center_axis',(-0.63706251599997,-0.770812137104617,0.)) ;
#12563 = DIRECTION('ref_axis',(0.770812137104617,-0.63706251599997,0.)) ;
#12564 = DIRECTION('',(0.770812137104617,-0.63706251599997,0.)) ;
#12565 = DIRECTION('center_axis',(0.,0.,1.)) ;
#12566 = DIRECTION('ref_axis',(0.939692620785908,-0.342020143325669,0.)) ;
#12567 = DIRECTION('center_axis',(0.,0.,1.)) ;
#12568 = DIRECTION('ref_axis',(1.,0.,0.)) ;
#12569 = DIRECTION('center_axis',(0.,0.,1.)) ;
#12570 = DIRECTION('ref_axis',(1.,0.,0.)) ;
#12571 = DIRECTION('',(-0.707106781186542,8.65956056235487E-17,0.707106781186553)) ;
#12572 = DIRECTION('center_axis',(0.,0.,1.)) ;
#12573 = DIRECTION('ref_axis',(0.866025403784438,-0.5,0.)) ;
#12574 = DIRECTION('',(0.648477023773232,-0.761234227842003,0.)) ;
#12575 = DIRECTION('',(-0.983486691428025,0.180980462437127,0.)) ;
#12576 = DIRECTION('center_axis',(0.180980462437127,0.983486691428025,0.)) ;
#12577 = DIRECTION('ref_axis',(-0.983486691428025,0.180980462437127,0.)) ;
#12578 = DIRECTION('',(0.,0.,1.)) ;
#12579 = DIRECTION('center_axis',(-0.761234227842003,-0.648477023773232,0.)) ;
#12580 = DIRECTION('ref_axis',(0.648477023773232,-0.761234227842003,0.)) ;
#12581 = DIRECTION('center_axis',(0.349011634277972,0.937118391207119,0.)) ;
#12582 = DIRECTION('ref_axis',(-0.937118391207119,0.349011634277972,0.)) ;
#12583 = DIRECTION('',(-0.937118391207119,0.349011634277972,0.)) ;
#12584 = DIRECTION('',(0.,0.,1.)) ;
#12585 = DIRECTION('center_axis',(-0.862276222874163,-0.506438264219704,0.)) ;
#12586 = DIRECTION('ref_axis',(0.506438264219704,-0.862276222874163,0.)) ;
#12587 = DIRECTION('',(0.506438264219704,-0.862276222874163,0.)) ;
#12588 = DIRECTION('center_axis',(0.,0.,1.)) ;
#12589 = DIRECTION('ref_axis',(0.766044443118978,-0.64278760968654,0.)) ;
#12590 = DIRECTION('center_axis',(0.,0.,1.)) ;
#12591 = DIRECTION('ref_axis',(0.642787609686539,-0.766044443118978,0.)) ;
#12592 = DIRECTION('',(0.349011634277988,-0.937118391207113,0.)) ;
#12593 = DIRECTION('',(-0.862276222874171,0.50643826421969,0.)) ;
#12594 = DIRECTION('center_axis',(0.50643826421969,0.862276222874171,0.)) ;
#12595 = DIRECTION('ref_axis',(-0.862276222874171,0.50643826421969,0.)) ;
#12596 = DIRECTION('',(0.,0.,1.)) ;
#12597 = DIRECTION('center_axis',(-0.937118391207113,-0.349011634277988,0.)) ;
#12598 = DIRECTION('ref_axis',(0.349011634277988,-0.937118391207113,0.)) ;
#12599 = DIRECTION('center_axis',(0.648477023773219,0.761234227842014,0.)) ;
#12600 = DIRECTION('ref_axis',(-0.761234227842014,0.648477023773219,0.)) ;
#12601 = DIRECTION('',(-0.761234227842014,0.648477023773219,0.)) ;
#12602 = DIRECTION('',(0.,0.,1.)) ;
#12603 = DIRECTION('center_axis',(-0.983486691428022,-0.180980462437143,0.)) ;
#12604 = DIRECTION('ref_axis',(0.180980462437143,-0.983486691428022,0.)) ;
#12605 = DIRECTION('',(0.180980462437143,-0.983486691428022,0.)) ;
#12606 = DIRECTION('center_axis',(0.,0.,1.)) ;
#12607 = DIRECTION('ref_axis',(0.5,-0.866025403784439,0.)) ;
#12608 = DIRECTION('center_axis',(0.,0.,1.)) ;
#12609 = DIRECTION('ref_axis',(0.342020143325668,-0.939692620785909,0.)) ;
#12610 = DIRECTION('',(0.007450290825678,-0.99997224619817,0.)) ;
#12611 = DIRECTION('',(-0.637062515999983,0.770812137104607,0.)) ;
#12612 = DIRECTION('center_axis',(0.770812137104607,0.637062515999983,0.)) ;
#12613 = DIRECTION('ref_axis',(-0.637062515999983,0.770812137104607,0.)) ;
#12614 = DIRECTION('',(0.,0.,1.)) ;
#12615 = DIRECTION('center_axis',(-0.99997224619817,-0.007450290825678,0.)) ;
#12616 = DIRECTION('ref_axis',(0.007450290825678,-0.99997224619817,0.)) ;
#12617 = DIRECTION('center_axis',(0.869726513699833,0.49353398197848,0.)) ;
#12618 = DIRECTION('ref_axis',(-0.49353398197848,0.869726513699833,0.)) ;
#12619 = DIRECTION('',(-0.49353398197848,0.869726513699833,0.)) ;
#12620 = DIRECTION('',(0.,0.,1.)) ;
#12621 = DIRECTION('center_axis',(-0.986074150277958,0.166306254102496,0.)) ;
#12622 = DIRECTION('ref_axis',(-0.166306254102496,-0.986074150277958,0.)) ;
#12623 = DIRECTION('',(-0.166306254102496,-0.986074150277958,0.)) ;
#12624 = DIRECTION('center_axis',(0.,0.,1.)) ;
#12625 = DIRECTION('ref_axis',(0.17364817766693,-0.984807753012208,0.)) ;
#12626 = DIRECTION('center_axis',(0.,0.,1.)) ;
#12627 = DIRECTION('ref_axis',(-1.83697019872103E-16,-1.,0.)) ;
#12628 = DIRECTION('',(-0.33500966765479,-0.942214690279146,0.)) ;
#12629 = DIRECTION('',(-0.335009667654806,0.94221469027914,0.)) ;
#12630 = DIRECTION('center_axis',(0.94221469027914,0.335009667654806,0.)) ;
#12631 = DIRECTION('ref_axis',(-0.335009667654806,0.94221469027914,0.)) ;
#12632 = DIRECTION('',(0.,0.,1.)) ;
#12633 = DIRECTION('center_axis',(-0.942214690279146,0.33500966765479,0.)) ;
#12634 = DIRECTION('ref_axis',(-0.33500966765479,-0.942214690279146,0.)) ;
#12635 = DIRECTION('center_axis',(0.986074150277955,0.166306254102512,0.)) ;
#12636 = DIRECTION('ref_axis',(-0.166306254102512,0.986074150277955,0.)) ;
#12637 = DIRECTION('',(-0.166306254102512,0.986074150277955,0.)) ;
#12638 = DIRECTION('',(0.,0.,1.)) ;
#12639 = DIRECTION('center_axis',(-0.869726513699841,0.493533981978465,0.)) ;
#12640 = DIRECTION('ref_axis',(-0.493533981978465,-0.869726513699841,0.)) ;
#12641 = DIRECTION('',(-0.493533981978465,-0.869726513699841,0.)) ;
#12642 = DIRECTION('center_axis',(0.,0.,1.)) ;
#12643 = DIRECTION('ref_axis',(-0.17364817766693,-0.984807753012208,0.)) ;
#12644 = DIRECTION('center_axis',(0.,0.,1.)) ;
#12645 = DIRECTION('ref_axis',(-0.342020143325669,-0.939692620785908,0.)) ;
#12646 = DIRECTION('',(-0.63706251599997,-0.770812137104617,0.)) ;
#12647 = DIRECTION('',(0.00745029082566179,0.99997224619817,0.)) ;
#12648 = DIRECTION('center_axis',(0.99997224619817,-0.00745029082566179,0.)) ;
#12649 = DIRECTION('ref_axis',(0.00745029082566179,0.99997224619817,0.)) ;
#12650 = DIRECTION('',(0.,0.,1.)) ;
#12651 = DIRECTION('center_axis',(-0.770812137104617,0.63706251599997,0.)) ;
#12652 = DIRECTION('ref_axis',(-0.63706251599997,-0.770812137104617,0.)) ;
#12653 = DIRECTION('center_axis',(0.983486691428025,-0.180980462437127,0.)) ;
#12654 = DIRECTION('ref_axis',(0.180980462437127,0.983486691428025,0.)) ;
#12655 = DIRECTION('',(0.180980462437127,0.983486691428025,0.)) ;
#12656 = DIRECTION('',(0.,0.,1.)) ;
#12657 = DIRECTION('center_axis',(-0.648477023773232,0.761234227842003,0.)) ;
#12658 = DIRECTION('ref_axis',(-0.761234227842003,-0.648477023773232,0.)) ;
#12659 = DIRECTION('',(-0.761234227842003,-0.648477023773232,0.)) ;
#12660 = DIRECTION('center_axis',(0.,0.,1.)) ;
#12661 = DIRECTION('ref_axis',(-0.5,-0.866025403784438,0.)) ;
#12662 = DIRECTION('center_axis',(0.,0.,1.)) ;
#12663 = DIRECTION('ref_axis',(-0.642787609686539,-0.766044443118978,0.)) ;
#12664 = DIRECTION('',(-0.862276222874163,-0.506438264219704,0.)) ;
#12665 = DIRECTION('',(0.349011634277972,0.937118391207119,0.)) ;
#12666 = DIRECTION('center_axis',(0.937118391207119,-0.349011634277972,0.)) ;
#12667 = DIRECTION('ref_axis',(0.349011634277972,0.937118391207119,0.)) ;
#12668 = DIRECTION('',(0.,0.,1.)) ;
#12669 = DIRECTION('center_axis',(-0.506438264219705,0.862276222874163,0.)) ;
#12670 = DIRECTION('ref_axis',(-0.862276222874163,-0.506438264219704,0.)) ;
#12671 = DIRECTION('center_axis',(0.862276222874172,-0.50643826421969,0.)) ;
#12672 = DIRECTION('ref_axis',(0.50643826421969,0.862276222874171,0.)) ;
#12673 = DIRECTION('',(0.50643826421969,0.862276222874171,0.)) ;
#12674 = DIRECTION('',(0.,0.,1.)) ;
#12675 = DIRECTION('center_axis',(-0.349011634277988,0.937118391207113,0.)) ;
#12676 = DIRECTION('ref_axis',(-0.937118391207113,-0.349011634277988,0.)) ;
#12677 = DIRECTION('',(-0.937118391207113,-0.349011634277988,0.)) ;
#12678 = DIRECTION('center_axis',(0.,0.,1.)) ;
#12679 = DIRECTION('ref_axis',(-0.766044443118978,-0.642787609686539,0.)) ;
#12680 = DIRECTION('center_axis',(0.,0.,1.)) ;
#12681 = DIRECTION('ref_axis',(-0.866025403784439,-0.5,0.)) ;
#12682 = DIRECTION('',(-0.983486691428022,-0.180980462437143,0.)) ;
#12683 = DIRECTION('',(0.648477023773219,0.761234227842014,0.)) ;
#12684 = DIRECTION('center_axis',(0.761234227842014,-0.648477023773219,0.)) ;
#12685 = DIRECTION('ref_axis',(0.648477023773219,0.761234227842014,0.)) ;
#12686 = DIRECTION('',(0.,0.,1.)) ;
#12687 = DIRECTION('center_axis',(-0.180980462437143,0.983486691428022,0.)) ;
#12688 = DIRECTION('ref_axis',(-0.983486691428022,-0.180980462437143,0.)) ;
#12689 = DIRECTION('center_axis',(0.637062515999983,-0.770812137104607,0.)) ;
#12690 = DIRECTION('ref_axis',(0.770812137104607,0.637062515999983,0.)) ;
#12691 = DIRECTION('',(0.770812137104607,0.637062515999983,0.)) ;
#12692 = DIRECTION('',(0.,0.,1.)) ;
#12693 = DIRECTION('center_axis',(-0.00745029082567855,0.99997224619817,0.)) ;
#12694 = DIRECTION('ref_axis',(-0.99997224619817,-0.00745029082567855,0.)) ;
#12695 = DIRECTION('',(-0.99997224619817,-0.00745029082567855,0.)) ;
#12696 = DIRECTION('center_axis',(0.,0.,1.)) ;
#12697 = DIRECTION('ref_axis',(-0.939692620785909,-0.342020143325669,0.)) ;
#12698 = DIRECTION('center_axis',(0.,0.,1.)) ;
#12699 = DIRECTION('ref_axis',(-0.984807753012208,-0.17364817766693,0.)) ;
#12700 = DIRECTION('',(-0.986074150277958,0.166306254102495,0.)) ;
#12701 = DIRECTION('',(0.869726513699833,0.49353398197848,0.)) ;
#12702 = DIRECTION('center_axis',(0.49353398197848,-0.869726513699833,0.)) ;
#12703 = DIRECTION('ref_axis',(0.869726513699833,0.49353398197848,0.)) ;
#12704 = DIRECTION('',(0.,0.,1.)) ;
#12705 = DIRECTION('center_axis',(0.166306254102495,0.986074150277958,0.)) ;
#12706 = DIRECTION('ref_axis',(-0.986074150277958,0.166306254102495,0.)) ;
#12707 = DIRECTION('center_axis',(0.335009667654806,-0.94221469027914,0.)) ;
#12708 = DIRECTION('ref_axis',(0.94221469027914,0.335009667654806,0.)) ;
#12709 = DIRECTION('',(0.94221469027914,0.335009667654806,0.)) ;
#12710 = DIRECTION('',(0.,0.,1.)) ;
#12711 = DIRECTION('center_axis',(0.33500966765479,0.942214690279146,0.)) ;
#12712 = DIRECTION('ref_axis',(-0.942214690279146,0.33500966765479,0.)) ;
#12713 = DIRECTION('',(-0.942214690279146,0.33500966765479,0.)) ;
#12714 = DIRECTION('center_axis',(0.,0.,1.)) ;
#12715 = DIRECTION('ref_axis',(-1.,1.22464679914735E-16,0.)) ;
#12716 = DIRECTION('center_axis',(0.,0.,1.)) ;
#12717 = DIRECTION('ref_axis',(-0.984807753012208,0.173648177666931,0.)) ;
#12718 = DIRECTION('',(-0.869726513699841,0.493533981978465,0.)) ;
#12719 = DIRECTION('',(0.986074150277955,0.166306254102512,0.)) ;
#12720 = DIRECTION('center_axis',(0.166306254102512,-0.986074150277955,0.)) ;
#12721 = DIRECTION('ref_axis',(0.986074150277955,0.166306254102512,0.)) ;
#12722 = DIRECTION('',(0.,0.,1.)) ;
#12723 = DIRECTION('center_axis',(0.493533981978465,0.869726513699841,0.)) ;
#12724 = DIRECTION('ref_axis',(-0.869726513699841,0.493533981978465,0.)) ;
#12725 = DIRECTION('center_axis',(-0.00745029082566129,-0.99997224619817,
0.)) ;
#12726 = DIRECTION('ref_axis',(0.99997224619817,-0.00745029082566129,0.)) ;
#12727 = DIRECTION('',(0.99997224619817,-0.00745029082566129,0.)) ;
#12728 = DIRECTION('',(0.,0.,1.)) ;
#12729 = DIRECTION('center_axis',(0.63706251599997,0.770812137104618,0.)) ;
#12730 = DIRECTION('ref_axis',(-0.770812137104618,0.63706251599997,0.)) ;
#12731 = DIRECTION('',(-0.770812137104618,0.63706251599997,0.)) ;
#12732 = DIRECTION('center_axis',(0.,0.,1.)) ;
#12733 = DIRECTION('ref_axis',(-0.939692620785908,0.342020143325669,0.)) ;
#12734 = DIRECTION('center_axis',(0.,0.,1.)) ;
#12735 = DIRECTION('ref_axis',(-0.866025403784439,0.5,0.)) ;
#12736 = DIRECTION('',(-0.648477023773233,0.761234227842003,0.)) ;
#12737 = DIRECTION('',(0.983486691428025,-0.180980462437126,0.)) ;
#12738 = DIRECTION('center_axis',(-0.180980462437126,-0.983486691428025,0.)) ;
#12739 = DIRECTION('ref_axis',(0.983486691428025,-0.180980462437126,0.)) ;
#12740 = DIRECTION('',(0.,0.,1.)) ;
#12741 = DIRECTION('center_axis',(0.761234227842003,0.648477023773233,0.)) ;
#12742 = DIRECTION('ref_axis',(-0.648477023773233,0.761234227842003,0.)) ;
#12743 = DIRECTION('center_axis',(-0.349011634277972,-0.937118391207119,0.)) ;
#12744 = DIRECTION('ref_axis',(0.937118391207119,-0.349011634277972,0.)) ;
#12745 = DIRECTION('',(0.937118391207119,-0.349011634277972,0.)) ;
#12746 = DIRECTION('',(0.,0.,1.)) ;
#12747 = DIRECTION('center_axis',(0.862276222874163,0.506438264219705,0.)) ;
#12748 = DIRECTION('ref_axis',(-0.506438264219704,0.862276222874163,0.)) ;
#12749 = DIRECTION('',(-0.506438264219704,0.862276222874163,0.)) ;
#12750 = DIRECTION('center_axis',(0.,0.,1.)) ;
#12751 = DIRECTION('ref_axis',(-0.766044443118978,0.642787609686539,0.)) ;
#12752 = DIRECTION('center_axis',(0.,0.,1.)) ;
#12753 = DIRECTION('ref_axis',(-0.642787609686539,0.766044443118978,0.)) ;
#12754 = DIRECTION('',(-0.349011634277988,0.937118391207113,0.)) ;
#12755 = DIRECTION('',(0.862276222874171,-0.506438264219689,0.)) ;
#12756 = DIRECTION('center_axis',(-0.50643826421969,-0.862276222874172,0.)) ;
#12757 = DIRECTION('ref_axis',(0.862276222874171,-0.506438264219689,0.)) ;
#12758 = DIRECTION('',(0.,0.,1.)) ;
#12759 = DIRECTION('center_axis',(0.937118391207113,0.349011634277988,0.)) ;
#12760 = DIRECTION('ref_axis',(-0.349011634277988,0.937118391207113,0.)) ;
#12761 = DIRECTION('center_axis',(-0.648477023773219,-0.761234227842014,0.)) ;
#12762 = DIRECTION('ref_axis',(0.761234227842014,-0.648477023773219,0.)) ;
#12763 = DIRECTION('',(0.761234227842014,-0.648477023773219,0.)) ;
#12764 = DIRECTION('',(0.,0.,1.)) ;
#12765 = DIRECTION('center_axis',(0.983486691428022,0.180980462437143,0.)) ;
#12766 = DIRECTION('ref_axis',(-0.180980462437143,0.983486691428022,0.)) ;
#12767 = DIRECTION('',(-0.180980462437143,0.983486691428022,0.)) ;
#12768 = DIRECTION('center_axis',(0.,0.,1.)) ;
#12769 = DIRECTION('ref_axis',(-0.5,0.866025403784439,0.)) ;
#12770 = DIRECTION('center_axis',(0.,0.,1.)) ;
#12771 = DIRECTION('ref_axis',(-0.342020143325669,0.939692620785908,0.)) ;
#12772 = DIRECTION('',(-0.00745029082567861,0.99997224619817,0.)) ;
#12773 = DIRECTION('',(0.637062515999983,-0.770812137104607,0.)) ;
#12774 = DIRECTION('center_axis',(-0.770812137104607,-0.637062515999983,0.)) ;
#12775 = DIRECTION('ref_axis',(0.637062515999983,-0.770812137104607,0.)) ;
#12776 = DIRECTION('',(0.,0.,1.)) ;
#12777 = DIRECTION('center_axis',(0.99997224619817,0.00745029082567861,0.)) ;
#12778 = DIRECTION('ref_axis',(-0.00745029082567861,0.99997224619817,0.)) ;
#12779 = DIRECTION('center_axis',(-0.869726513699833,-0.49353398197848,0.)) ;
#12780 = DIRECTION('ref_axis',(0.49353398197848,-0.869726513699833,0.)) ;
#12781 = DIRECTION('',(0.49353398197848,-0.869726513699833,0.)) ;
#12782 = DIRECTION('',(0.,0.,1.)) ;
#12783 = DIRECTION('center_axis',(0.986074150277958,-0.166306254102495,0.)) ;
#12784 = DIRECTION('ref_axis',(0.166306254102495,0.986074150277958,0.)) ;
#12785 = DIRECTION('',(0.166306254102495,0.986074150277958,0.)) ;
#12786 = DIRECTION('center_axis',(0.,0.,1.)) ;
#12787 = DIRECTION('ref_axis',(-0.17364817766693,0.984807753012208,0.)) ;
#12788 = DIRECTION('center_axis',(0.,0.,1.)) ;
#12789 = DIRECTION('ref_axis',(6.12323399573677E-17,1.,0.)) ;
#12790 = DIRECTION('',(0.33500966765479,0.942214690279146,0.)) ;
#12791 = DIRECTION('',(0.335009667654806,-0.94221469027914,0.)) ;
#12792 = DIRECTION('center_axis',(-0.94221469027914,-0.335009667654806,0.)) ;
#12793 = DIRECTION('ref_axis',(0.335009667654806,-0.94221469027914,0.)) ;
#12794 = DIRECTION('',(0.,0.,1.)) ;
#12795 = DIRECTION('center_axis',(0.942214690279146,-0.33500966765479,0.)) ;
#12796 = DIRECTION('ref_axis',(0.33500966765479,0.942214690279146,0.)) ;
#12797 = DIRECTION('center_axis',(-0.986074150277955,-0.166306254102512,0.)) ;
#12798 = DIRECTION('ref_axis',(0.166306254102512,-0.986074150277955,0.)) ;
#12799 = DIRECTION('',(0.166306254102512,-0.986074150277955,0.)) ;
#12800 = DIRECTION('',(0.,0.,1.)) ;
#12801 = DIRECTION('center_axis',(0.869726513699841,-0.493533981978465,0.)) ;
#12802 = DIRECTION('ref_axis',(0.493533981978465,0.869726513699841,0.)) ;
#12803 = DIRECTION('',(0.493533981978465,0.869726513699841,0.)) ;
#12804 = DIRECTION('center_axis',(0.,0.,1.)) ;
#12805 = DIRECTION('ref_axis',(0.17364817766693,0.984807753012208,0.)) ;
#12806 = DIRECTION('center_axis',(0.,0.,1.)) ;
#12807 = DIRECTION('ref_axis',(0.342020143325669,0.939692620785908,0.)) ;
#12808 = DIRECTION('',(0.63706251599997,0.770812137104618,0.)) ;
#12809 = DIRECTION('',(-0.00745029082566129,-0.99997224619817,0.)) ;
#12810 = DIRECTION('center_axis',(-0.99997224619817,0.00745029082566129,0.)) ;
#12811 = DIRECTION('ref_axis',(-0.00745029082566129,-0.99997224619817,0.)) ;
#12812 = DIRECTION('',(0.,0.,1.)) ;
#12813 = DIRECTION('center_axis',(0.770812137104618,-0.63706251599997,0.)) ;
#12814 = DIRECTION('ref_axis',(0.63706251599997,0.770812137104618,0.)) ;
#12815 = DIRECTION('center_axis',(-0.983486691428025,0.180980462437126,0.)) ;
#12816 = DIRECTION('ref_axis',(-0.180980462437126,-0.983486691428025,0.)) ;
#12817 = DIRECTION('',(-0.180980462437126,-0.983486691428025,0.)) ;
#12818 = DIRECTION('',(0.,0.,1.)) ;
#12819 = DIRECTION('center_axis',(0.648477023773232,-0.761234227842003,0.)) ;
#12820 = DIRECTION('ref_axis',(0.761234227842003,0.648477023773232,0.)) ;
#12821 = DIRECTION('',(0.761234227842003,0.648477023773232,0.)) ;
#12822 = DIRECTION('center_axis',(0.,0.,1.)) ;
#12823 = DIRECTION('ref_axis',(0.5,0.866025403784439,0.)) ;
#12824 = DIRECTION('center_axis',(0.,0.,1.)) ;
#12825 = DIRECTION('ref_axis',(0.642787609686539,0.766044443118978,0.)) ;
#12826 = DIRECTION('',(0.862276222874163,0.506438264219705,0.)) ;
#12827 = DIRECTION('',(-0.349011634277972,-0.937118391207119,0.)) ;
#12828 = DIRECTION('center_axis',(-0.937118391207119,0.349011634277972,0.)) ;
#12829 = DIRECTION('ref_axis',(-0.349011634277972,-0.937118391207119,0.)) ;
#12830 = DIRECTION('',(0.,0.,1.)) ;
#12831 = DIRECTION('center_axis',(0.506438264219705,-0.862276222874163,0.)) ;
#12832 = DIRECTION('ref_axis',(0.862276222874163,0.506438264219705,0.)) ;
#12833 = DIRECTION('center_axis',(-0.862276222874172,0.50643826421969,0.)) ;
#12834 = DIRECTION('ref_axis',(-0.50643826421969,-0.862276222874171,0.)) ;
#12835 = DIRECTION('',(-0.50643826421969,-0.862276222874171,0.)) ;
#12836 = DIRECTION('',(0.,0.,1.)) ;
#12837 = DIRECTION('center_axis',(0.349011634277988,-0.937118391207113,0.)) ;
#12838 = DIRECTION('ref_axis',(0.937118391207113,0.349011634277988,0.)) ;
#12839 = DIRECTION('',(0.937118391207113,0.349011634277988,0.)) ;
#12840 = DIRECTION('center_axis',(0.,0.,1.)) ;
#12841 = DIRECTION('ref_axis',(0.766044443118978,0.642787609686539,0.)) ;
#12842 = DIRECTION('center_axis',(0.,0.,1.)) ;
#12843 = DIRECTION('ref_axis',(0.866025403784439,0.5,0.)) ;
#12844 = DIRECTION('',(0.983486691428022,0.180980462437143,0.)) ;
#12845 = DIRECTION('',(-0.648477023773219,-0.761234227842014,0.)) ;
#12846 = DIRECTION('center_axis',(-0.761234227842014,0.648477023773219,0.)) ;
#12847 = DIRECTION('ref_axis',(-0.648477023773219,-0.761234227842014,0.)) ;
#12848 = DIRECTION('',(0.,0.,1.)) ;
#12849 = DIRECTION('center_axis',(0.180980462437143,-0.983486691428022,0.)) ;
#12850 = DIRECTION('ref_axis',(0.983486691428022,0.180980462437143,0.)) ;
#12851 = DIRECTION('center_axis',(-0.637062515999983,0.770812137104607,0.)) ;
#12852 = DIRECTION('ref_axis',(-0.770812137104607,-0.637062515999983,0.)) ;
#12853 = DIRECTION('',(-0.770812137104607,-0.637062515999983,0.)) ;
#12854 = DIRECTION('',(0.,0.,1.)) ;
#12855 = DIRECTION('center_axis',(0.00745029082567861,-0.99997224619817,0.)) ;
#12856 = DIRECTION('ref_axis',(0.99997224619817,0.00745029082567861,0.)) ;
#12857 = DIRECTION('',(0.99997224619817,0.00745029082567861,0.)) ;
#12858 = DIRECTION('center_axis',(0.,0.,1.)) ;
#12859 = DIRECTION('ref_axis',(0.939692620785908,0.342020143325669,0.)) ;
#12860 = DIRECTION('center_axis',(0.,0.,1.)) ;
#12861 = DIRECTION('ref_axis',(0.984807753012208,0.17364817766693,0.)) ;
#12862 = DIRECTION('',(0.986074150277958,-0.166306254102495,0.)) ;
#12863 = DIRECTION('',(-0.869726513699833,-0.49353398197848,0.)) ;
#12864 = DIRECTION('center_axis',(-0.49353398197848,0.869726513699833,0.)) ;
#12865 = DIRECTION('ref_axis',(-0.869726513699833,-0.49353398197848,0.)) ;
#12866 = DIRECTION('',(0.,0.,1.)) ;
#12867 = DIRECTION('center_axis',(-0.166306254102495,-0.986074150277958,0.)) ;
#12868 = DIRECTION('ref_axis',(0.986074150277958,-0.166306254102495,0.)) ;
#12869 = DIRECTION('center_axis',(-0.335009667654806,0.94221469027914,0.)) ;
#12870 = DIRECTION('ref_axis',(-0.94221469027914,-0.335009667654806,0.)) ;
#12871 = DIRECTION('',(-0.94221469027914,-0.335009667654806,0.)) ;
#12872 = DIRECTION('',(0.,0.,1.)) ;
#12873 = DIRECTION('center_axis',(-0.33500966765479,-0.942214690279146,0.)) ;
#12874 = DIRECTION('ref_axis',(0.942214690279146,-0.33500966765479,0.)) ;
#12875 = DIRECTION('',(0.942214690279146,-0.33500966765479,0.)) ;
#12876 = DIRECTION('center_axis',(0.,0.,1.)) ;
#12877 = DIRECTION('ref_axis',(1.,0.,0.)) ;
#12878 = DIRECTION('center_axis',(0.,0.,1.)) ;
#12879 = DIRECTION('ref_axis',(1.,0.,0.)) ;
#12880 = DIRECTION('center_axis',(0.,-1.,0.)) ;
#12881 = DIRECTION('ref_axis',(-1.,0.,0.)) ;
#12882 = DIRECTION('center_axis',(0.,0.,1.)) ;
#12883 = DIRECTION('ref_axis',(1.,0.,0.)) ;
#12884 = DIRECTION('center_axis',(0.,0.,1.)) ;
#12885 = DIRECTION('ref_axis',(1.,0.,0.)) ;
#12886 = DIRECTION('center_axis',(0.,0.,-1.)) ;
#12887 = DIRECTION('ref_axis',(1.,0.,0.)) ;
#12888 = DIRECTION('',(0.70710678118654,8.65956056235484E-17,0.707106781186555)) ;
#12889 = DIRECTION('center_axis',(0.,0.,1.)) ;
#12890 = DIRECTION('ref_axis',(1.,0.,0.)) ;
#12891 = DIRECTION('center_axis',(0.,0.,1.)) ;
#12892 = DIRECTION('ref_axis',(1.,0.,0.)) ;
#12893 = DIRECTION('center_axis',(0.,0.,1.)) ;
#12894 = DIRECTION('ref_axis',(1.,0.,0.)) ;
#12895 = DIRECTION('center_axis',(0.,0.,1.)) ;
#12896 = DIRECTION('ref_axis',(1.,0.,0.)) ;
#12897 = DIRECTION('center_axis',(0.,0.,1.)) ;
#12898 = DIRECTION('ref_axis',(1.,0.,0.)) ;
#12899 = DIRECTION('center_axis',(0.,0.,1.)) ;
#12900 = DIRECTION('ref_axis',(1.,0.,0.)) ;
#12901 = DIRECTION('center_axis',(0.,0.,1.)) ;
#12902 = DIRECTION('ref_axis',(1.,0.,0.)) ;
#12903 = DIRECTION('',(0.,0.,-1.)) ;
#12904 = DIRECTION('',(0.,0.,1.)) ;
#12905 = DIRECTION('center_axis',(0.,0.,-1.)) ;
#12906 = DIRECTION('ref_axis',(1.,0.,0.)) ;
#12907 = DIRECTION('center_axis',(0.,0.,1.)) ;
#12908 = DIRECTION('ref_axis',(1.,0.,0.)) ;
#12909 = DIRECTION('',(0.,0.,-1.)) ;
#12910 = DIRECTION('',(0.,0.,1.)) ;
#12911 = DIRECTION('center_axis',(0.,0.,-1.)) ;
#12912 = DIRECTION('ref_axis',(1.,0.,0.)) ;
#12913 = DIRECTION('center_axis',(0.,0.,1.)) ;
#12914 = DIRECTION('ref_axis',(1.,0.,0.)) ;
#12915 = DIRECTION('',(0.,0.,1.)) ;
#12916 = DIRECTION('center_axis',(0.,0.,-1.)) ;
#12917 = DIRECTION('ref_axis',(1.,0.,0.)) ;
#12918 = DIRECTION('',(0.,0.,-1.)) ;
#12919 = DIRECTION('center_axis',(0.,0.,1.)) ;
#12920 = DIRECTION('ref_axis',(1.,0.,0.)) ;
#12921 = DIRECTION('',(0.,0.,-1.)) ;
#12922 = DIRECTION('',(0.,0.,1.)) ;
#12923 = DIRECTION('center_axis',(0.,0.,-1.)) ;
#12924 = DIRECTION('ref_axis',(1.,0.,0.)) ;
#12925 = DIRECTION('center_axis',(0.,0.,1.)) ;
#12926 = DIRECTION('ref_axis',(1.,0.,0.)) ;
#12927 = DIRECTION('',(0.,0.,1.)) ;
#12928 = DIRECTION('center_axis',(0.,0.,-1.)) ;
#12929 = DIRECTION('ref_axis',(1.,0.,0.)) ;
#12930 = DIRECTION('',(0.,0.,-1.)) ;
#12931 = DIRECTION('center_axis',(0.,0.,1.)) ;
#12932 = DIRECTION('ref_axis',(1.,0.,0.)) ;
#12933 = DIRECTION('',(0.,0.,1.)) ;
#12934 = DIRECTION('center_axis',(0.,0.,-1.)) ;
#12935 = DIRECTION('ref_axis',(1.,0.,0.)) ;
#12936 = DIRECTION('',(0.,0.,-1.)) ;
#12937 = DIRECTION('center_axis',(0.,1.,0.)) ;
#12938 = DIRECTION('ref_axis',(-1.,0.,0.)) ;
#12939 = DIRECTION('',(-1.,0.,0.)) ;
#12940 = DIRECTION('',(0.,0.,1.)) ;
#12941 = DIRECTION('',(-1.,0.,0.)) ;
#12942 = DIRECTION('',(0.,0.,1.)) ;
#12943 = DIRECTION('center_axis',(0.866025403784449,0.499999999999982,0.)) ;
#12944 = DIRECTION('ref_axis',(-0.499999999999982,0.866025403784449,0.)) ;
#12945 = DIRECTION('',(-0.499999999999982,0.866025403784449,0.)) ;
#12946 = DIRECTION('',(0.,0.,1.)) ;
#12947 = DIRECTION('',(-0.499999999999982,0.866025403784449,0.)) ;
#12948 = DIRECTION('center_axis',(0.866025403784449,-0.499999999999982,0.)) ;
#12949 = DIRECTION('ref_axis',(0.499999999999982,0.866025403784449,0.)) ;
#12950 = DIRECTION('',(0.499999999999982,0.866025403784449,0.)) ;
#12951 = DIRECTION('',(0.,0.,1.)) ;
#12952 = DIRECTION('',(0.499999999999982,0.866025403784449,0.)) ;
#12953 = DIRECTION('center_axis',(0.,0.,1.)) ;
#12954 = DIRECTION('ref_axis',(1.,0.,0.)) ;
#12955 = DIRECTION('center_axis',(0.,0.,1.)) ;
#12956 = DIRECTION('ref_axis',(1.,0.,0.)) ;
#12957 = DIRECTION('center_axis',(0.,0.,1.)) ;
#12958 = DIRECTION('ref_axis',(1.,0.,0.)) ;
#12959 = DIRECTION('',(1.,0.,0.)) ;
#12960 = DIRECTION('center_axis',(0.,0.,1.)) ;
#12961 = DIRECTION('ref_axis',(1.,0.,0.)) ;
#12962 = DIRECTION('center_axis',(0.,0.,1.)) ;
#12963 = DIRECTION('ref_axis',(1.,0.,0.)) ;
#12964 = DIRECTION('',(0.499999999999997,-0.86602540378444,0.)) ;
#12965 = DIRECTION('center_axis',(0.,0.,1.)) ;
#12966 = DIRECTION('ref_axis',(1.,0.,0.)) ;
#12967 = DIRECTION('',(-0.499999999999997,-0.86602540378444,0.)) ;
#12968 = DIRECTION('center_axis',(0.,0.,-1.)) ;
#12969 = DIRECTION('ref_axis',(-1.,0.,0.)) ;
#12970 = DIRECTION('',(1.,0.,0.)) ;
#12971 = DIRECTION('center_axis',(0.,0.,1.)) ;
#12972 = DIRECTION('ref_axis',(1.,0.,0.)) ;
#12973 = DIRECTION('center_axis',(0.,0.,-1.)) ;
#12974 = DIRECTION('ref_axis',(-1.,0.,0.)) ;
#12975 = DIRECTION('center_axis',(0.,0.,1.)) ;
#12976 = DIRECTION('ref_axis',(1.,0.,0.)) ;
#12977 = DIRECTION('center_axis',(0.,0.,-1.)) ;
#12978 = DIRECTION('ref_axis',(-1.,0.,0.)) ;
#12979 = DIRECTION('center_axis',(0.,0.,1.)) ;
#12980 = DIRECTION('ref_axis',(1.,0.,0.)) ;
#12981 = DIRECTION('center_axis',(0.,0.,-1.)) ;
#12982 = DIRECTION('ref_axis',(-1.,0.,0.)) ;
#12983 = DIRECTION('center_axis',(0.,0.,1.)) ;
#12984 = DIRECTION('ref_axis',(1.,0.,0.)) ;
#12985 = DIRECTION('center_axis',(0.,0.,-1.)) ;
#12986 = DIRECTION('ref_axis',(-1.,0.,0.)) ;
#12987 = DIRECTION('',(-0.499999999999997,-0.86602540378444,0.)) ;
#12988 = DIRECTION('center_axis',(0.,0.,1.)) ;
#12989 = DIRECTION('ref_axis',(1.,0.,0.)) ;
#12990 = DIRECTION('center_axis',(0.,0.,-1.)) ;
#12991 = DIRECTION('ref_axis',(-1.,0.,0.)) ;
#12992 = DIRECTION('',(0.499999999999997,-0.86602540378444,0.)) ;
#12993 = DIRECTION('center_axis',(0.,0.,1.)) ;
#12994 = DIRECTION('ref_axis',(1.,0.,0.)) ;
#12995 = DIRECTION('center_axis',(0.,0.,-1.)) ;
#12996 = DIRECTION('ref_axis',(1.,0.,0.)) ;
#12997 = DIRECTION('',(0.857167300702111,1.04972719113862E-16,0.515038074910056)) ;
#12998 = DIRECTION('center_axis',(0.,-1.,0.)) ;
#12999 = DIRECTION('ref_axis',(1.,0.,0.)) ;
#13000 = DIRECTION('',(0.,0.,1.)) ;
#13001 = DIRECTION('center_axis',(-0.86602540378444,-0.499999999999997,0.)) ;
#13002 = DIRECTION('ref_axis',(0.499999999999997,-0.86602540378444,0.)) ;
#13003 = DIRECTION('',(0.,0.,1.)) ;
#13004 = DIRECTION('center_axis',(-0.86602540378444,0.499999999999997,0.)) ;
#13005 = DIRECTION('ref_axis',(-0.499999999999997,-0.86602540378444,0.)) ;
#13006 = DIRECTION('axis',(0.,0.,1.)) ;
#13007 = DIRECTION('refdir',(1.,0.,0.)) ;
#13008 = DIRECTION('center_axis',(0.,0.,-1.)) ;
#13009 = DIRECTION('ref_axis',(1.,0.,0.)) ;
#13010 = DIRECTION('center_axis',(0.,0.,-1.)) ;
#13011 = DIRECTION('ref_axis',(1.,0.,0.)) ;
#13012 = DIRECTION('',(0.,0.,-1.)) ;
#13013 = DIRECTION('center_axis',(0.,0.,1.)) ;
#13014 = DIRECTION('ref_axis',(1.,0.,0.)) ;
#13015 = DIRECTION('center_axis',(0.,0.,-1.)) ;
#13016 = DIRECTION('ref_axis',(1.,0.,0.)) ;
#13017 = DIRECTION('center_axis',(0.,0.,-1.)) ;
#13018 = DIRECTION('ref_axis',(1.,0.,0.)) ;
#13019 = DIRECTION('',(0.,0.,-1.)) ;
#13020 = DIRECTION('center_axis',(0.,0.,1.)) ;
#13021 = DIRECTION('ref_axis',(1.,0.,0.)) ;
#13022 = DIRECTION('center_axis',(0.,0.,1.)) ;
#13023 = DIRECTION('ref_axis',(1.,0.,0.)) ;
#13024 = DIRECTION('center_axis',(0.,0.,1.)) ;
#13025 = DIRECTION('ref_axis',(1.,0.,0.)) ;
#13026 = DIRECTION('',(1.,0.,0.)) ;
#13027 = DIRECTION('',(0.,1.,0.)) ;
#13028 = DIRECTION('',(1.,0.,0.)) ;
#13029 = DIRECTION('',(0.,1.,0.)) ;
#13030 = DIRECTION('',(1.,0.,0.)) ;
#13031 = DIRECTION('center_axis',(0.,1.,0.)) ;
#13032 = DIRECTION('ref_axis',(1.,0.,0.)) ;
#13033 = DIRECTION('center_axis',(0.,-1.,0.)) ;
#13034 = DIRECTION('ref_axis',(1.,0.,0.)) ;
#13035 = DIRECTION('',(0.,-1.,0.)) ;
#13036 = DIRECTION('center_axis',(0.,-1.,0.)) ;
#13037 = DIRECTION('ref_axis',(1.,0.,0.)) ;
#13038 = DIRECTION('center_axis',(-1.,0.,0.)) ;
#13039 = DIRECTION('ref_axis',(0.,0.,1.)) ;
#13040 = DIRECTION('',(0.,0.,1.)) ;
#13041 = DIRECTION('',(0.,0.,1.)) ;
#13042 = DIRECTION('',(0.,1.,0.)) ;
#13043 = DIRECTION('center_axis',(0.,1.,0.)) ;
#13044 = DIRECTION('ref_axis',(1.,0.,1.33226762955019E-15)) ;
#13045 = DIRECTION('center_axis',(0.,1.,0.)) ;
#13046 = DIRECTION('ref_axis',(1.,0.,1.33226762955019E-15)) ;
#13047 = DIRECTION('center_axis',(0.,1.,0.)) ;
#13048 = DIRECTION('ref_axis',(1.,0.,1.33226762955019E-15)) ;
#13049 = DIRECTION('',(0.,1.,0.)) ;
#13050 = DIRECTION('center_axis',(1.,0.,0.)) ;
#13051 = DIRECTION('ref_axis',(0.,0.,-1.)) ;
#13052 = DIRECTION('',(0.,0.,-1.)) ;
#13053 = DIRECTION('',(0.,0.,-1.)) ;
#13054 = DIRECTION('center_axis',(0.,1.,0.)) ;
#13055 = DIRECTION('ref_axis',(1.,0.,0.)) ;
#13056 = DIRECTION('',(0.,0.,-1.)) ;
#13057 = DIRECTION('',(0.,0.,1.)) ;
#13058 = DIRECTION('',(-1.,0.,0.)) ;
#13059 = DIRECTION('center_axis',(0.,1.,0.)) ;
#13060 = DIRECTION('ref_axis',(1.,0.,0.)) ;
#13061 = DIRECTION('center_axis',(0.,0.,-1.)) ;
#13062 = DIRECTION('ref_axis',(-1.,0.,0.)) ;
#13063 = DIRECTION('center_axis',(0.,0.,1.)) ;
#13064 = DIRECTION('ref_axis',(1.,0.,0.)) ;
#13065 = DIRECTION('center_axis',(0.,0.,1.)) ;
#13066 = DIRECTION('ref_axis',(1.,0.,0.)) ;
#13067 = DIRECTION('',(1.,0.,0.)) ;
#13068 = DIRECTION('center_axis',(0.,0.,1.)) ;
#13069 = DIRECTION('ref_axis',(1.,0.,0.)) ;
#13070 = DIRECTION('center_axis',(0.,1.,0.)) ;
#13071 = DIRECTION('ref_axis',(1.,0.,0.)) ;
#13072 = DIRECTION('',(0.,0.,1.)) ;
#13073 = DIRECTION('',(0.,0.,-1.)) ;
#13074 = DIRECTION('',(1.,0.,0.)) ;
#13075 = DIRECTION('',(0.,0.,1.)) ;
#13076 = DIRECTION('center_axis',(0.,1.,0.)) ;
#13077 = DIRECTION('ref_axis',(1.,0.,1.33226762955019E-15)) ;
#13078 = DIRECTION('',(0.,0.,-1.)) ;
#13079 = DIRECTION('',(1.,0.,0.)) ;
#13080 = DIRECTION('center_axis',(0.,-1.,0.)) ;
#13081 = DIRECTION('ref_axis',(1.,0.,0.)) ;
#13082 = DIRECTION('center_axis',(0.,1.,0.)) ;
#13083 = DIRECTION('ref_axis',(1.,0.,0.)) ;
#13084 = DIRECTION('center_axis',(0.,-1.,0.)) ;
#13085 = DIRECTION('ref_axis',(1.,0.,0.)) ;
#13086 = DIRECTION('',(0.,-1.,0.)) ;
#13087 = DIRECTION('center_axis',(-1.,0.,0.)) ;
#13088 = DIRECTION('ref_axis',(0.,0.,1.)) ;
#13089 = DIRECTION('',(0.,1.,0.)) ;
#13090 = DIRECTION('',(0.,0.,1.)) ;
#13091 = DIRECTION('',(0.,1.,0.)) ;
#13092 = DIRECTION('center_axis',(0.,1.,0.)) ;
#13093 = DIRECTION('ref_axis',(1.,0.,1.33226762955019E-15)) ;
#13094 = DIRECTION('center_axis',(0.,1.,0.)) ;
#13095 = DIRECTION('ref_axis',(1.,0.,1.33226762955019E-15)) ;
#13096 = DIRECTION('',(0.,1.,0.)) ;
#13097 = DIRECTION('center_axis',(1.,0.,0.)) ;
#13098 = DIRECTION('ref_axis',(0.,0.,-1.)) ;
#13099 = DIRECTION('',(0.,0.,-1.)) ;
#13100 = DIRECTION('',(0.,1.,0.)) ;
#13101 = DIRECTION('center_axis',(0.,0.,1.)) ;
#13102 = DIRECTION('ref_axis',(1.,0.,0.)) ;
#13103 = DIRECTION('center_axis',(0.,0.,1.)) ;
#13104 = DIRECTION('ref_axis',(1.,0.,0.)) ;
#13105 = DIRECTION('',(1.,0.,0.)) ;
#13106 = DIRECTION('center_axis',(0.,1.,0.)) ;
#13107 = DIRECTION('ref_axis',(1.,0.,0.)) ;
#13108 = DIRECTION('center_axis',(0.,0.,1.)) ;
#13109 = DIRECTION('ref_axis',(1.,0.,0.)) ;
#13110 = DIRECTION('center_axis',(0.,0.,1.)) ;
#13111 = DIRECTION('ref_axis',(1.,0.,0.)) ;
#13112 = DIRECTION('',(0.,0.,-1.)) ;
#13113 = DIRECTION('center_axis',(0.,0.,-1.)) ;
#13114 = DIRECTION('ref_axis',(-1.,0.,0.)) ;
#13115 = DIRECTION('center_axis',(0.,0.,1.)) ;
#13116 = DIRECTION('ref_axis',(1.,0.,0.)) ;
#13117 = DIRECTION('center_axis',(0.,0.,1.)) ;
#13118 = DIRECTION('ref_axis',(1.,0.,0.)) ;
#13119 = DIRECTION('',(0.,0.,1.)) ;
#13120 = DIRECTION('center_axis',(0.,0.,-1.)) ;
#13121 = DIRECTION('ref_axis',(1.,0.,0.)) ;
#13122 = DIRECTION('center_axis',(0.,1.,0.)) ;
#13123 = DIRECTION('ref_axis',(-1.,0.,0.)) ;
#13124 = DIRECTION('',(-1.,0.,0.)) ;
#13125 = DIRECTION('',(0.,0.,1.)) ;
#13126 = DIRECTION('',(-1.,0.,0.)) ;
#13127 = DIRECTION('',(0.,0.,1.)) ;
#13128 = DIRECTION('center_axis',(1.,0.,0.)) ;
#13129 = DIRECTION('ref_axis',(0.,1.,0.)) ;
#13130 = DIRECTION('',(0.,1.,0.)) ;
#13131 = DIRECTION('',(0.,1.,0.)) ;
#13132 = DIRECTION('',(0.,0.,1.)) ;
#13133 = DIRECTION('center_axis',(0.,-1.,0.)) ;
#13134 = DIRECTION('ref_axis',(1.,0.,0.)) ;
#13135 = DIRECTION('',(1.,0.,0.)) ;
#13136 = DIRECTION('',(1.,0.,0.)) ;
#13137 = DIRECTION('',(0.,0.,1.)) ;
#13138 = DIRECTION('center_axis',(-1.,0.,0.)) ;
#13139 = DIRECTION('ref_axis',(0.,-1.,0.)) ;
#13140 = DIRECTION('',(0.,-1.,0.)) ;
#13141 = DIRECTION('',(0.,-1.,0.)) ;
#13142 = DIRECTION('center_axis',(0.,0.,1.)) ;
#13143 = DIRECTION('ref_axis',(1.,0.,0.)) ;
#13144 = DIRECTION('center_axis',(0.,0.,1.)) ;
#13145 = DIRECTION('ref_axis',(1.,0.,0.)) ;
#13146 = DIRECTION('axis',(0.,0.,1.)) ;
#13147 = DIRECTION('refdir',(1.,0.,0.)) ;
#13148 = DIRECTION('center_axis',(0.,0.,-1.)) ;
#13149 = DIRECTION('ref_axis',(1.,0.,0.)) ;
#13150 = DIRECTION('center_axis',(0.,0.,-1.)) ;
#13151 = DIRECTION('ref_axis',(1.,0.,0.)) ;
#13152 = DIRECTION('',(0.,0.,-1.)) ;
#13153 = DIRECTION('center_axis',(0.,0.,1.)) ;
#13154 = DIRECTION('ref_axis',(1.,0.,0.)) ;
#13155 = DIRECTION('center_axis',(0.,0.,-1.)) ;
#13156 = DIRECTION('ref_axis',(1.,0.,0.)) ;
#13157 = DIRECTION('center_axis',(0.,0.,-1.)) ;
#13158 = DIRECTION('ref_axis',(1.,0.,0.)) ;
#13159 = DIRECTION('',(0.,0.,-1.)) ;
#13160 = DIRECTION('center_axis',(0.,0.,1.)) ;
#13161 = DIRECTION('ref_axis',(1.,0.,0.)) ;
#13162 = DIRECTION('center_axis',(0.,1.,0.)) ;
#13163 = DIRECTION('ref_axis',(1.,0.,0.)) ;
#13164 = DIRECTION('',(-1.,0.,0.)) ;
#13165 = DIRECTION('',(0.,0.,-1.)) ;
#13166 = DIRECTION('center_axis',(0.,1.,0.)) ;
#13167 = DIRECTION('ref_axis',(1.,0.,1.33226762955019E-15)) ;
#13168 = DIRECTION('',(0.,0.,1.)) ;
#13169 = DIRECTION('center_axis',(0.,-1.,0.)) ;
#13170 = DIRECTION('ref_axis',(1.,0.,0.)) ;
#13171 = DIRECTION('center_axis',(1.,0.,0.)) ;
#13172 = DIRECTION('ref_axis',(0.,0.,-1.)) ;
#13173 = DIRECTION('',(0.,1.,0.)) ;
#13174 = DIRECTION('',(0.,0.,-1.)) ;
#13175 = DIRECTION('',(0.,1.,0.)) ;
#13176 = DIRECTION('center_axis',(0.,1.,0.)) ;
#13177 = DIRECTION('ref_axis',(1.,0.,0.)) ;
#13178 = DIRECTION('',(0.,-1.,0.)) ;
#13179 = DIRECTION('center_axis',(0.,-1.,0.)) ;
#13180 = DIRECTION('ref_axis',(1.,0.,0.)) ;
#13181 = DIRECTION('center_axis',(-1.,0.,0.)) ;
#13182 = DIRECTION('ref_axis',(0.,0.,1.)) ;
#13183 = DIRECTION('',(0.,-1.,0.)) ;
#13184 = DIRECTION('',(0.,1.,0.)) ;
#13185 = DIRECTION('',(0.,0.,1.)) ;
#13186 = DIRECTION('center_axis',(0.,1.,0.)) ;
#13187 = DIRECTION('ref_axis',(1.,0.,1.33226762955019E-15)) ;
#13188 = DIRECTION('center_axis',(0.,1.,0.)) ;
#13189 = DIRECTION('ref_axis',(1.,0.,1.33226762955019E-15)) ;
#13190 = DIRECTION('center_axis',(0.,1.,0.)) ;
#13191 = DIRECTION('ref_axis',(1.,0.,0.)) ;
#13192 = DIRECTION('',(1.,0.,0.)) ;
#13193 = DIRECTION('center_axis',(0.,1.,0.)) ;
#13194 = DIRECTION('ref_axis',(1.,0.,0.)) ;
#13195 = DIRECTION('',(-1.,0.,0.)) ;
#13196 = DIRECTION('',(0.,0.,-1.)) ;
#13197 = DIRECTION('center_axis',(0.,1.,0.)) ;
#13198 = DIRECTION('ref_axis',(1.,0.,1.33226762955019E-15)) ;
#13199 = DIRECTION('',(0.,0.,1.)) ;
#13200 = DIRECTION('center_axis',(0.,-1.,0.)) ;
#13201 = DIRECTION('ref_axis',(1.,0.,0.)) ;
#13202 = DIRECTION('center_axis',(1.,0.,0.)) ;
#13203 = DIRECTION('ref_axis',(0.,0.,-1.)) ;
#13204 = DIRECTION('',(0.,1.,0.)) ;
#13205 = DIRECTION('',(0.,0.,-1.)) ;
#13206 = DIRECTION('',(0.,1.,0.)) ;
#13207 = DIRECTION('center_axis',(0.,1.,0.)) ;
#13208 = DIRECTION('ref_axis',(1.,0.,0.)) ;
#13209 = DIRECTION('',(0.,-1.,0.)) ;
#13210 = DIRECTION('center_axis',(0.,-1.,0.)) ;
#13211 = DIRECTION('ref_axis',(1.,0.,0.)) ;
#13212 = DIRECTION('center_axis',(-1.,0.,0.)) ;
#13213 = DIRECTION('ref_axis',(0.,0.,1.)) ;
#13214 = DIRECTION('',(0.,-1.,0.)) ;
#13215 = DIRECTION('',(0.,1.,0.)) ;
#13216 = DIRECTION('',(0.,0.,1.)) ;
#13217 = DIRECTION('center_axis',(0.,1.,0.)) ;
#13218 = DIRECTION('ref_axis',(1.,0.,1.33226762955019E-15)) ;
#13219 = DIRECTION('center_axis',(0.,1.,0.)) ;
#13220 = DIRECTION('ref_axis',(1.,0.,1.33226762955019E-15)) ;
#13221 = DIRECTION('center_axis',(0.,1.,0.)) ;
#13222 = DIRECTION('ref_axis',(1.,0.,0.)) ;
#13223 = DIRECTION('',(1.,0.,0.)) ;
#13224 = DIRECTION('center_axis',(0.,1.,0.)) ;
#13225 = DIRECTION('ref_axis',(-1.,0.,0.)) ;
#13226 = DIRECTION('',(-1.,0.,0.)) ;
#13227 = DIRECTION('',(0.,0.,1.)) ;
#13228 = DIRECTION('',(-1.,0.,0.)) ;
#13229 = DIRECTION('',(0.,0.,1.)) ;
#13230 = DIRECTION('center_axis',(1.,0.,0.)) ;
#13231 = DIRECTION('ref_axis',(0.,1.,0.)) ;
#13232 = DIRECTION('',(0.,1.,0.)) ;
#13233 = DIRECTION('',(0.,1.,0.)) ;
#13234 = DIRECTION('',(0.,0.,1.)) ;
#13235 = DIRECTION('center_axis',(0.,-1.,0.)) ;
#13236 = DIRECTION('ref_axis',(1.,0.,0.)) ;
#13237 = DIRECTION('',(1.,0.,0.)) ;
#13238 = DIRECTION('',(1.,0.,0.)) ;
#13239 = DIRECTION('',(0.,0.,1.)) ;
#13240 = DIRECTION('center_axis',(-1.,0.,0.)) ;
#13241 = DIRECTION('ref_axis',(0.,-1.,0.)) ;
#13242 = DIRECTION('',(0.,-1.,0.)) ;
#13243 = DIRECTION('',(0.,-1.,0.)) ;
#13244 = DIRECTION('center_axis',(0.,0.,1.)) ;
#13245 = DIRECTION('ref_axis',(1.,0.,0.)) ;
#13246 = DIRECTION('center_axis',(0.,0.,1.)) ;
#13247 = DIRECTION('ref_axis',(1.,0.,0.)) ;
#13248 = DIRECTION('axis',(0.,0.,1.)) ;
#13249 = DIRECTION('refdir',(1.,0.,0.)) ;
#13250 = DIRECTION('center_axis',(0.,1.,0.)) ;
#13251 = DIRECTION('ref_axis',(0.,0.,1.)) ;
#13252 = DIRECTION('center_axis',(0.,-1.,0.)) ;
#13253 = DIRECTION('ref_axis',(1.,0.,0.)) ;
#13254 = DIRECTION('center_axis',(0.,-1.,0.)) ;
#13255 = DIRECTION('ref_axis',(1.,0.,0.)) ;
#13256 = DIRECTION('center_axis',(0.,-1.,0.)) ;
#13257 = DIRECTION('ref_axis',(1.,0.,0.)) ;
#13258 = DIRECTION('center_axis',(0.,-1.,0.)) ;
#13259 = DIRECTION('ref_axis',(1.,0.,0.)) ;
#13260 = DIRECTION('',(0.,1.,0.)) ;
#13261 = DIRECTION('center_axis',(0.,1.,0.)) ;
#13262 = DIRECTION('ref_axis',(0.,0.,1.)) ;
#13263 = DIRECTION('center_axis',(0.,-1.,0.)) ;
#13264 = DIRECTION('ref_axis',(1.,0.,0.)) ;
#13265 = DIRECTION('center_axis',(0.,-1.,0.)) ;
#13266 = DIRECTION('ref_axis',(1.,0.,0.)) ;
#13267 = DIRECTION('center_axis',(0.,-1.,0.)) ;
#13268 = DIRECTION('ref_axis',(1.,0.,0.)) ;
#13269 = DIRECTION('',(0.919145030018058,0.393919298579168,1.12562801896381E-16)) ;
#13270 = DIRECTION('center_axis',(0.,-1.,0.)) ;
#13271 = DIRECTION('ref_axis',(1.,0.,0.)) ;
#13272 = DIRECTION('center_axis',(0.,-1.,0.)) ;
#13273 = DIRECTION('ref_axis',(1.,0.,0.)) ;
#13274 = DIRECTION('',(0.737154140200746,0.675724628517341,9.02753458275063E-17)) ;
#13275 = DIRECTION('center_axis',(0.,-1.,0.)) ;
#13276 = DIRECTION('ref_axis',(1.,0.,0.)) ;
#13277 = DIRECTION('center_axis',(0.,-1.,0.)) ;
#13278 = DIRECTION('ref_axis',(1.,0.,0.)) ;
#13279 = DIRECTION('',(0.,1.,0.)) ;
#13280 = DIRECTION('center_axis',(0.,1.,0.)) ;
#13281 = DIRECTION('ref_axis',(1.,0.,0.)) ;
#13282 = DIRECTION('center_axis',(0.,-1.,0.)) ;
#13283 = DIRECTION('ref_axis',(1.,0.,0.)) ;
#13284 = DIRECTION('',(-0.737154140200746,0.675724628517341,-9.02753458275063E-17)) ;
#13285 = DIRECTION('center_axis',(0.,1.,0.)) ;
#13286 = DIRECTION('ref_axis',(1.,0.,0.)) ;
#13287 = DIRECTION('center_axis',(0.,-1.,0.)) ;
#13288 = DIRECTION('ref_axis',(1.,0.,0.)) ;
#13289 = DIRECTION('',(-0.919145030018055,0.393919298579173,-1.12562801896381E-16)) ;
#13290 = DIRECTION('center_axis',(0.,-1.,0.)) ;
#13291 = DIRECTION('ref_axis',(0.,0.,-1.)) ;
#13292 = DIRECTION('center_axis',(0.,-1.,0.)) ;
#13293 = DIRECTION('ref_axis',(1.,0.,0.)) ;
#13294 = DIRECTION('center_axis',(0.,-1.,0.)) ;
#13295 = DIRECTION('ref_axis',(1.,0.,0.)) ;
#13296 = DIRECTION('center_axis',(0.,-1.,0.)) ;
#13297 = DIRECTION('ref_axis',(1.,0.,0.)) ;
#13298 = DIRECTION('',(0.,1.,0.)) ;
#13299 = DIRECTION('center_axis',(0.,-1.,0.)) ;
#13300 = DIRECTION('ref_axis',(0.,0.,-1.)) ;
#13301 = DIRECTION('center_axis',(0.,-1.,0.)) ;
#13302 = DIRECTION('ref_axis',(1.,0.,0.)) ;
#13303 = DIRECTION('center_axis',(0.,-1.,0.)) ;
#13304 = DIRECTION('ref_axis',(1.,0.,0.)) ;
#13305 = DIRECTION('',(0.,1.,0.)) ;
#13306 = DIRECTION('',(0.,0.,1.)) ;
#13307 = DIRECTION('',(1.,0.,0.)) ;
#13308 = DIRECTION('',(0.,0.,1.)) ;
#13309 = DIRECTION('',(1.,0.,0.)) ;
#13310 = DIRECTION('',(0.832757238017344,0.,0.553638313820245)) ;
#13311 = DIRECTION('',(0.553638313820245,0.,-0.832757238017344)) ;
#13312 = DIRECTION('',(-0.832757238017344,0.,0.553638313820245)) ;
#13313 = DIRECTION('',(0.553638313820245,0.,0.832757238017344)) ;
#13314 = DIRECTION('',(0.,0.,1.)) ;
#13315 = DIRECTION('',(1.,0.,0.)) ;
#13316 = DIRECTION('',(0.,0.,1.)) ;
#13317 = DIRECTION('',(1.,0.,0.)) ;
#13318 = DIRECTION('',(0.,0.,1.)) ;
#13319 = DIRECTION('',(1.,0.,0.)) ;
#13320 = DIRECTION('',(0.895942659405472,0.,0.444169732261722)) ;
#13321 = DIRECTION('',(0.444169732261722,0.,-0.895942659405472)) ;
#13322 = DIRECTION('',(0.895942659405472,0.,0.444169732261722)) ;
#13323 = DIRECTION('',(0.444169732261722,0.,-0.895942659405472)) ;
#13324 = DIRECTION('',(0.,0.,1.)) ;
#13325 = DIRECTION('',(1.,0.,0.)) ;
#13326 = DIRECTION('',(0.,0.,1.)) ;
#13327 = DIRECTION('',(1.,0.,0.)) ;
#13328 = DIRECTION('',(0.,0.,1.)) ;
#13329 = DIRECTION('',(1.,0.,0.)) ;
#13330 = DIRECTION('',(0.,0.,1.)) ;
#13331 = DIRECTION('',(1.,0.,0.)) ;
#13332 = DIRECTION('',(0.,0.,1.)) ;
#13333 = DIRECTION('',(1.,0.,0.)) ;
#13334 = DIRECTION('',(0.,0.,1.)) ;
#13335 = DIRECTION('',(1.,0.,0.)) ;
#13336 = DIRECTION('',(0.,0.,1.)) ;
#13337 = DIRECTION('',(1.,0.,0.)) ;
#13338 = DIRECTION('',(0.,0.,1.)) ;
#13339 = DIRECTION('',(1.,0.,0.)) ;
#13340 = DIRECTION('',(0.,0.,-1.)) ;
#13341 = DIRECTION('',(1.,0.,0.)) ;
#13342 = DIRECTION('',(0.,0.,-1.)) ;
#13343 = DIRECTION('',(1.,0.,0.)) ;
#13344 = DIRECTION('',(0.,0.,1.)) ;
#13345 = DIRECTION('',(1.,0.,0.)) ;
#13346 = DIRECTION('',(0.,0.,1.)) ;
#13347 = DIRECTION('',(1.,0.,0.)) ;
#13348 = DIRECTION('',(0.,0.,-1.)) ;
#13349 = DIRECTION('',(1.,0.,0.)) ;
#13350 = DIRECTION('',(0.,0.,-1.)) ;
#13351 = DIRECTION('',(1.,0.,0.)) ;
#13352 = DIRECTION('',(0.,0.,1.)) ;
#13353 = DIRECTION('',(1.,0.,0.)) ;
#13354 = DIRECTION('',(0.,0.,1.)) ;
#13355 = DIRECTION('',(1.,0.,0.)) ;
#13356 = DIRECTION('',(0.,0.,-1.)) ;
#13357 = DIRECTION('',(1.,0.,0.)) ;
#13358 = DIRECTION('',(0.,0.,-1.)) ;
#13359 = DIRECTION('',(1.,0.,0.)) ;
#13360 = DIRECTION('',(0.,0.,1.)) ;
#13361 = DIRECTION('',(1.,0.,0.)) ;
#13362 = DIRECTION('',(0.,0.,1.)) ;
#13363 = DIRECTION('',(1.,0.,0.)) ;
#13364 = DIRECTION('',(0.,0.,1.)) ;
#13365 = DIRECTION('',(1.,0.,0.)) ;
#13366 = DIRECTION('',(0.,0.,1.)) ;
#13367 = DIRECTION('',(1.,0.,0.)) ;
#13368 = DIRECTION('',(0.,0.,1.)) ;
#13369 = DIRECTION('',(1.,0.,0.)) ;
#13370 = DIRECTION('',(0.,0.,1.)) ;
#13371 = DIRECTION('',(1.,0.,0.)) ;
#13372 = DIRECTION('',(0.,0.,1.)) ;
#13373 = DIRECTION('',(1.,0.,0.)) ;
#13374 = DIRECTION('',(0.,0.,1.)) ;
#13375 = DIRECTION('',(1.,0.,0.)) ;
#13376 = DIRECTION('',(0.,0.,-1.)) ;
#13377 = DIRECTION('',(1.,0.,0.)) ;
#13378 = DIRECTION('',(0.,0.,-1.)) ;
#13379 = DIRECTION('',(1.,0.,0.)) ;
#13380 = DIRECTION('',(0.,0.,1.)) ;
#13381 = DIRECTION('',(1.,0.,0.)) ;
#13382 = DIRECTION('',(0.,0.,1.)) ;
#13383 = DIRECTION('',(1.,0.,0.)) ;
#13384 = DIRECTION('',(0.,0.,-1.)) ;
#13385 = DIRECTION('',(1.,0.,0.)) ;
#13386 = DIRECTION('',(0.,0.,-1.)) ;
#13387 = DIRECTION('',(1.,0.,0.)) ;
#13388 = DIRECTION('',(0.,0.,-1.)) ;
#13389 = DIRECTION('',(1.,0.,0.)) ;
#13390 = DIRECTION('',(0.,0.,-1.)) ;
#13391 = DIRECTION('',(1.,0.,0.)) ;
#13392 = DIRECTION('',(0.,0.,1.)) ;
#13393 = DIRECTION('',(1.,0.,0.)) ;
#13394 = DIRECTION('',(0.,0.,1.)) ;
#13395 = DIRECTION('',(1.,0.,0.)) ;
#13396 = DIRECTION('',(0.,0.,1.)) ;
#13397 = DIRECTION('',(1.,0.,0.)) ;
#13398 = DIRECTION('',(0.,0.,1.)) ;
#13399 = DIRECTION('',(1.,0.,0.)) ;
#13400 = DIRECTION('',(0.,0.,1.)) ;
#13401 = DIRECTION('',(1.,0.,0.)) ;
#13402 = DIRECTION('',(0.,0.,1.)) ;
#13403 = DIRECTION('',(1.,0.,0.)) ;
#13404 = DIRECTION('',(0.,0.,1.)) ;
#13405 = DIRECTION('',(1.,0.,0.)) ;
#13406 = DIRECTION('',(0.,0.,1.)) ;
#13407 = DIRECTION('',(1.,0.,0.)) ;
#13408 = DIRECTION('',(-1.,0.,0.)) ;
#13409 = DIRECTION('',(0.,0.,1.)) ;
#13410 = DIRECTION('',(-1.,0.,0.)) ;
#13411 = DIRECTION('',(0.,0.,1.)) ;
#13412 = DIRECTION('',(0.,0.,1.)) ;
#13413 = DIRECTION('',(-1.,1.22464679914735E-16,0.)) ;
#13414 = DIRECTION('',(0.,0.,1.)) ;
#13415 = DIRECTION('',(-1.,1.22464679914735E-16,0.)) ;
#13416 = DIRECTION('',(0.,0.,1.)) ;
#13417 = DIRECTION('',(-1.,1.22464679914735E-16,0.)) ;
#13418 = DIRECTION('',(0.,0.,1.)) ;
#13419 = DIRECTION('',(1.,0.,0.)) ;
#13420 = DIRECTION('',(0.,0.,1.)) ;
#13421 = DIRECTION('',(-1.,1.22464679914735E-16,0.)) ;
#13422 = CARTESIAN_POINT('',(0.,0.,0.)) ;
#13423 = CARTESIAN_POINT('',(0.,0.,0.)) ;
#13424 = CARTESIAN_POINT('Origin',(-84.75,-52.3,27.675)) ;
#13425 = CARTESIAN_POINT('',(-85.95,-52.3,27.6)) ;
#13426 = CARTESIAN_POINT('Origin',(-84.75,-52.3,27.6)) ;
#13427 = CARTESIAN_POINT('',(-85.8,-52.3,27.75)) ;
#13428 = CARTESIAN_POINT('',(-85.875,-52.3,27.675)) ;
#13429 = CARTESIAN_POINT('Origin',(-84.75,-52.3,27.75)) ;
#13430 = CARTESIAN_POINT('Origin',(-78.25,-52.3,27.6)) ;
#13431 = CARTESIAN_POINT('',(-87.25,-45.3,27.6)) ;
#13432 = CARTESIAN_POINT('',(-87.25,-59.3,27.6)) ;
#13433 = CARTESIAN_POINT('',(-87.25,-45.3,27.6)) ;
#13434 = CARTESIAN_POINT('',(-69.25,-45.3,27.6)) ;
#13435 = CARTESIAN_POINT('',(-69.25,-45.3,27.6)) ;
#13436 = CARTESIAN_POINT('',(-69.25,-59.3,27.6)) ;
#13437 = CARTESIAN_POINT('',(-69.25,-59.3,27.6)) ;
#13438 = CARTESIAN_POINT('',(-87.25,-59.3,27.6)) ;
#13439 = CARTESIAN_POINT('',(-72.95,-52.3,27.6)) ;
#13440 = CARTESIAN_POINT('Origin',(-71.75,-52.3,27.6)) ;
#13441 = CARTESIAN_POINT('Origin',(-84.75,-52.3,27.6)) ;
#13442 = CARTESIAN_POINT('',(-85.8,-52.3,33.4)) ;
#13443 = CARTESIAN_POINT('',(-85.8,-52.3,27.6)) ;
#13444 = CARTESIAN_POINT('Origin',(-84.75,-52.3,33.4)) ;
#13445 = CARTESIAN_POINT('Origin',(-84.75,52.3,27.675)) ;
#13446 = CARTESIAN_POINT('',(-85.95,52.3,27.6)) ;
#13447 = CARTESIAN_POINT('Origin',(-84.75,52.3,27.6)) ;
#13448 = CARTESIAN_POINT('',(-85.8,52.3,27.75)) ;
#13449 = CARTESIAN_POINT('',(-85.875,52.3,27.675)) ;
#13450 = CARTESIAN_POINT('Origin',(-84.75,52.3,27.75)) ;
#13451 = CARTESIAN_POINT('Origin',(-78.25,52.3,27.6)) ;
#13452 = CARTESIAN_POINT('',(-87.25,59.3,27.6)) ;
#13453 = CARTESIAN_POINT('',(-87.25,45.3,27.6)) ;
#13454 = CARTESIAN_POINT('',(-87.25,59.3,27.6)) ;
#13455 = CARTESIAN_POINT('',(-69.25,59.3,27.6)) ;
#13456 = CARTESIAN_POINT('',(-69.25,59.3,27.6)) ;
#13457 = CARTESIAN_POINT('',(-69.25,45.3,27.6)) ;
#13458 = CARTESIAN_POINT('',(-69.25,45.3,27.6)) ;
#13459 = CARTESIAN_POINT('',(-87.25,45.3,27.6)) ;
#13460 = CARTESIAN_POINT('',(-72.95,52.3,27.6)) ;
#13461 = CARTESIAN_POINT('Origin',(-71.75,52.3,27.6)) ;
#13462 = CARTESIAN_POINT('Origin',(-84.75,52.3,27.6)) ;
#13463 = CARTESIAN_POINT('',(-85.8,52.3,33.4)) ;
#13464 = CARTESIAN_POINT('',(-85.8,52.3,27.6)) ;
#13465 = CARTESIAN_POINT('Origin',(-84.75,52.3,33.4)) ;
#13466 = CARTESIAN_POINT('Origin',(84.75,52.3,27.675)) ;
#13467 = CARTESIAN_POINT('',(83.55,52.3,27.6)) ;
#13468 = CARTESIAN_POINT('Origin',(84.75,52.3,27.6)) ;
#13469 = CARTESIAN_POINT('',(83.7,52.3,27.75)) ;
#13470 = CARTESIAN_POINT('',(83.625,52.3,27.675)) ;
#13471 = CARTESIAN_POINT('Origin',(84.75,52.3,27.75)) ;
#13472 = CARTESIAN_POINT('Origin',(78.25,52.3,27.6)) ;
#13473 = CARTESIAN_POINT('',(69.25,59.3,27.6)) ;
#13474 = CARTESIAN_POINT('',(69.25,45.3,27.6)) ;
#13475 = CARTESIAN_POINT('',(69.25,59.3,27.6)) ;
#13476 = CARTESIAN_POINT('',(87.25,59.3,27.6)) ;
#13477 = CARTESIAN_POINT('',(87.25,59.3,27.6)) ;
#13478 = CARTESIAN_POINT('',(87.25,45.3,27.6)) ;
#13479 = CARTESIAN_POINT('',(87.25,45.3,27.6)) ;
#13480 = CARTESIAN_POINT('',(69.25,45.3,27.6)) ;
#13481 = CARTESIAN_POINT('',(70.55,52.3,27.6)) ;
#13482 = CARTESIAN_POINT('Origin',(71.75,52.3,27.6)) ;
#13483 = CARTESIAN_POINT('Origin',(84.75,52.3,27.6)) ;
#13484 = CARTESIAN_POINT('',(83.7,52.3,33.4)) ;
#13485 = CARTESIAN_POINT('',(83.7,52.3,27.6)) ;
#13486 = CARTESIAN_POINT('Origin',(84.75,52.3,33.4)) ;
#13487 = CARTESIAN_POINT('Origin',(84.75,-52.3,27.675)) ;
#13488 = CARTESIAN_POINT('',(83.55,-52.3,27.6)) ;
#13489 = CARTESIAN_POINT('Origin',(84.75,-52.3,27.6)) ;
#13490 = CARTESIAN_POINT('',(83.7,-52.3,27.75)) ;
#13491 = CARTESIAN_POINT('',(83.625,-52.3,27.675)) ;
#13492 = CARTESIAN_POINT('Origin',(84.75,-52.3,27.75)) ;
#13493 = CARTESIAN_POINT('Origin',(78.25,-52.3,27.6)) ;
#13494 = CARTESIAN_POINT('',(69.25,-45.3,27.6)) ;
#13495 = CARTESIAN_POINT('',(69.25,-59.3,27.6)) ;
#13496 = CARTESIAN_POINT('',(69.25,-45.3,27.6)) ;
#13497 = CARTESIAN_POINT('',(87.25,-45.3,27.6)) ;
#13498 = CARTESIAN_POINT('',(87.25,-45.3,27.6)) ;
#13499 = CARTESIAN_POINT('',(87.25,-59.3,27.6)) ;
#13500 = CARTESIAN_POINT('',(87.25,-59.3,27.6)) ;
#13501 = CARTESIAN_POINT('',(69.25,-59.3,27.6)) ;
#13502 = CARTESIAN_POINT('',(70.55,-52.3,27.6)) ;
#13503 = CARTESIAN_POINT('Origin',(71.75,-52.3,27.6)) ;
#13504 = CARTESIAN_POINT('Origin',(84.75,-52.3,27.6)) ;
#13505 = CARTESIAN_POINT('',(83.7,-52.3,33.4)) ;
#13506 = CARTESIAN_POINT('',(83.7,-52.3,27.6)) ;
#13507 = CARTESIAN_POINT('Origin',(84.75,-52.3,33.4)) ;
#13508 = CARTESIAN_POINT('Origin',(71.75,52.3,27.675)) ;
#13509 = CARTESIAN_POINT('',(70.7,52.3,27.75)) ;
#13510 = CARTESIAN_POINT('',(70.625,52.3,27.675)) ;
#13511 = CARTESIAN_POINT('Origin',(71.75,52.3,27.75)) ;
#13512 = CARTESIAN_POINT('Origin',(71.75,52.3,27.6)) ;
#13513 = CARTESIAN_POINT('',(70.7,52.3,33.4)) ;
#13514 = CARTESIAN_POINT('',(70.7,52.3,27.6)) ;
#13515 = CARTESIAN_POINT('',(70.7183994382024,52.1042954244305,33.4)) ;
#13516 = CARTESIAN_POINT('Origin',(71.75,52.3,33.4)) ;
#13517 = CARTESIAN_POINT('',(70.7183994382024,52.4957045755694,33.4)) ;
#13518 = CARTESIAN_POINT('Ctrl Pts',(70.7183994382024,52.4957045755694,33.4)) ;
#13519 = CARTESIAN_POINT('Ctrl Pts',(70.7319761095756,52.5672701062946,33.389125081463)) ;
#13520 = CARTESIAN_POINT('Ctrl Pts',(70.7531407522362,52.6376371859408,33.3724123738805)) ;
#13521 = CARTESIAN_POINT('Ctrl Pts',(70.8341056071048,52.8316627295715,33.3125298347947)) ;
#13522 = CARTESIAN_POINT('Ctrl Pts',(70.9124422905779,52.9458062688949,33.2592888082397)) ;
#13523 = CARTESIAN_POINT('Ctrl Pts',(71.0924279408069,53.128845249026,33.1588871128703)) ;
#13524 = CARTESIAN_POINT('Ctrl Pts',(71.2082663884949,53.2104458534536,33.1040987390693)) ;
#13525 = CARTESIAN_POINT('Ctrl Pts',(71.4676871756213,53.3211202136295,33.0155789759107)) ;
#13526 = CARTESIAN_POINT('Ctrl Pts',(71.611512060708,53.35,32.98231678229)) ;
#13527 = CARTESIAN_POINT('Ctrl Pts',(71.8811502184983,53.35,32.9491868010911)) ;
#13528 = CARTESIAN_POINT('Ctrl Pts',(72.021484418179,53.3238190465072,32.9460485518659)) ;
#13529 = CARTESIAN_POINT('Ctrl Pts',(72.2790771456966,53.2175982662943,32.9649830273315)) ;
#13530 = CARTESIAN_POINT('Ctrl Pts',(72.3964053699774,53.1376182539018,32.9864379744825)) ;
#13531 = CARTESIAN_POINT('Ctrl Pts',(72.5827722667432,52.9530317340365,33.0322038118174)) ;
#13532 = CARTESIAN_POINT('Ctrl Pts',(72.6641459041156,52.835355369045,33.0596974322278)) ;
#13533 = CARTESIAN_POINT('Ctrl Pts',(72.7727880560022,52.5759934056159,33.1003519438363)) ;
#13534 = CARTESIAN_POINT('Ctrl Pts',(72.8,52.4341327809988,33.1125413911823)) ;
#13535 = CARTESIAN_POINT('Ctrl Pts',(72.8,52.3,33.1125413911823)) ;
#13536 = CARTESIAN_POINT('Ctrl Pts',(72.8,52.1658672190012,33.1125413911823)) ;
#13537 = CARTESIAN_POINT('Ctrl Pts',(72.7727880560022,52.0240065943841,33.1003519438363)) ;
#13538 = CARTESIAN_POINT('Ctrl Pts',(72.6641459041156,51.764644630955,33.0596974322278)) ;
#13539 = CARTESIAN_POINT('Ctrl Pts',(72.5827722667432,51.6469682659635,33.0322038118174)) ;
#13540 = CARTESIAN_POINT('Ctrl Pts',(72.3964053699774,51.4623817460982,32.9864379744825)) ;
#13541 = CARTESIAN_POINT('Ctrl Pts',(72.2790771456966,51.3824017337057,32.9649830273315)) ;
#13542 = CARTESIAN_POINT('Ctrl Pts',(72.021484418179,51.2761809534928,32.9460485518659)) ;
#13543 = CARTESIAN_POINT('Ctrl Pts',(71.8811502184983,51.25,32.9491868010911)) ;
#13544 = CARTESIAN_POINT('Ctrl Pts',(71.611512060708,51.25,32.98231678229)) ;
#13545 = CARTESIAN_POINT('Ctrl Pts',(71.4676871756213,51.2788797863705,33.0155789759107)) ;
#13546 = CARTESIAN_POINT('Ctrl Pts',(71.2082663884949,51.3895541465464,33.1040987390693)) ;
#13547 = CARTESIAN_POINT('Ctrl Pts',(71.0924279408069,51.471154750974,33.1588871128703)) ;
#13548 = CARTESIAN_POINT('Ctrl Pts',(70.9124422905779,51.6541937311051,33.2592888082397)) ;
#13549 = CARTESIAN_POINT('Ctrl Pts',(70.8341056071048,51.7683372704285,33.3125298347947)) ;
#13550 = CARTESIAN_POINT('Ctrl Pts',(70.7531407522363,51.9623628140592,33.3724123738805)) ;
#13551 = CARTESIAN_POINT('Ctrl Pts',(70.7319761095756,52.0327298937054,33.389125081463)) ;
#13552 = CARTESIAN_POINT('Ctrl Pts',(70.7183994382024,52.1042954244305,33.4)) ;
#13553 = CARTESIAN_POINT('Origin',(71.75,52.3,33.4)) ;
#13554 = CARTESIAN_POINT('Origin',(71.75,-52.3,27.675)) ;
#13555 = CARTESIAN_POINT('',(70.7,-52.3,27.75)) ;
#13556 = CARTESIAN_POINT('',(70.625,-52.3,27.675)) ;
#13557 = CARTESIAN_POINT('Origin',(71.75,-52.3,27.75)) ;
#13558 = CARTESIAN_POINT('Origin',(71.75,-52.3,27.6)) ;
#13559 = CARTESIAN_POINT('',(70.7,-52.3,33.4)) ;
#13560 = CARTESIAN_POINT('',(70.7,-52.3,27.6)) ;
#13561 = CARTESIAN_POINT('',(70.7183994382024,-52.4957045755694,33.4)) ;
#13562 = CARTESIAN_POINT('Origin',(71.75,-52.3,33.4)) ;
#13563 = CARTESIAN_POINT('',(70.7183994382024,-52.1042954244305,33.4)) ;
#13564 = CARTESIAN_POINT('Ctrl Pts',(70.7183994382024,-52.1042954244305,33.4)) ;
#13565 = CARTESIAN_POINT('Ctrl Pts',(70.7319761095756,-52.0327298937054,33.389125081463)) ;
#13566 = CARTESIAN_POINT('Ctrl Pts',(70.7531407522363,-51.9623628140592,33.3724123738805)) ;
#13567 = CARTESIAN_POINT('Ctrl Pts',(70.8341056071048,-51.7683372704285,33.3125298347947)) ;
#13568 = CARTESIAN_POINT('Ctrl Pts',(70.9124422905779,-51.6541937311051,33.2592888082397)) ;
#13569 = CARTESIAN_POINT('Ctrl Pts',(71.0924279408069,-51.471154750974,33.1588871128703)) ;
#13570 = CARTESIAN_POINT('Ctrl Pts',(71.2082663884949,-51.3895541465464,33.1040987390693)) ;
#13571 = CARTESIAN_POINT('Ctrl Pts',(71.4676871756213,-51.2788797863704,33.0155789759107)) ;
#13572 = CARTESIAN_POINT('Ctrl Pts',(71.611512060708,-51.25,32.98231678229)) ;
#13573 = CARTESIAN_POINT('Ctrl Pts',(71.8811502184983,-51.25,32.9491868010911)) ;
#13574 = CARTESIAN_POINT('Ctrl Pts',(72.021484418179,-51.2761809534928,32.9460485518659)) ;
#13575 = CARTESIAN_POINT('Ctrl Pts',(72.2790771456966,-51.3824017337057,32.9649830273315)) ;
#13576 = CARTESIAN_POINT('Ctrl Pts',(72.3964053699774,-51.4623817460982,32.9864379744825)) ;
#13577 = CARTESIAN_POINT('Ctrl Pts',(72.5827722667432,-51.6469682659635,33.0322038118174)) ;
#13578 = CARTESIAN_POINT('Ctrl Pts',(72.6641459041156,-51.764644630955,33.0596974322278)) ;
#13579 = CARTESIAN_POINT('Ctrl Pts',(72.7727880560022,-52.0240065943841,33.1003519438363)) ;
#13580 = CARTESIAN_POINT('Ctrl Pts',(72.8,-52.1658672190012,33.1125413911823)) ;
#13581 = CARTESIAN_POINT('Ctrl Pts',(72.8,-52.3,33.1125413911823)) ;
#13582 = CARTESIAN_POINT('Ctrl Pts',(72.8,-52.4341327809988,33.1125413911823)) ;
#13583 = CARTESIAN_POINT('Ctrl Pts',(72.7727880560022,-52.5759934056159,33.1003519438363)) ;
#13584 = CARTESIAN_POINT('Ctrl Pts',(72.6641459041156,-52.835355369045,33.0596974322278)) ;
#13585 = CARTESIAN_POINT('Ctrl Pts',(72.5827722667432,-52.9530317340365,33.0322038118174)) ;
#13586 = CARTESIAN_POINT('Ctrl Pts',(72.3964053699774,-53.1376182539018,32.9864379744825)) ;
#13587 = CARTESIAN_POINT('Ctrl Pts',(72.2790771456966,-53.2175982662943,32.9649830273315)) ;
#13588 = CARTESIAN_POINT('Ctrl Pts',(72.021484418179,-53.3238190465072,32.9460485518659)) ;
#13589 = CARTESIAN_POINT('Ctrl Pts',(71.8811502184983,-53.35,32.9491868010911)) ;
#13590 = CARTESIAN_POINT('Ctrl Pts',(71.611512060708,-53.35,32.98231678229)) ;
#13591 = CARTESIAN_POINT('Ctrl Pts',(71.4676871756213,-53.3211202136296,33.0155789759107)) ;
#13592 = CARTESIAN_POINT('Ctrl Pts',(71.2082663884949,-53.2104458534536,33.1040987390693)) ;
#13593 = CARTESIAN_POINT('Ctrl Pts',(71.0924279408069,-53.128845249026,33.1588871128703)) ;
#13594 = CARTESIAN_POINT('Ctrl Pts',(70.9124422905779,-52.9458062688949,33.2592888082397)) ;
#13595 = CARTESIAN_POINT('Ctrl Pts',(70.8341056071048,-52.8316627295715,33.3125298347947)) ;
#13596 = CARTESIAN_POINT('Ctrl Pts',(70.7531407522362,-52.6376371859408,33.3724123738805)) ;
#13597 = CARTESIAN_POINT('Ctrl Pts',(70.7319761095756,-52.5672701062946,33.389125081463)) ;
#13598 = CARTESIAN_POINT('Ctrl Pts',(70.7183994382024,-52.4957045755694,33.4)) ;
#13599 = CARTESIAN_POINT('Origin',(71.75,-52.3,33.4)) ;
#13600 = CARTESIAN_POINT('Origin',(-71.75,52.3,27.675)) ;
#13601 = CARTESIAN_POINT('',(-72.8,52.3,27.75)) ;
#13602 = CARTESIAN_POINT('',(-72.875,52.3,27.675)) ;
#13603 = CARTESIAN_POINT('Origin',(-71.75,52.3,27.75)) ;
#13604 = CARTESIAN_POINT('Origin',(-71.75,52.3,27.6)) ;
#13605 = CARTESIAN_POINT('',(-72.8,52.3,33.4)) ;
#13606 = CARTESIAN_POINT('',(-72.8,52.3,27.6)) ;
#13607 = CARTESIAN_POINT('Origin',(-71.75,52.3,33.4)) ;
#13608 = CARTESIAN_POINT('Origin',(-71.75,-52.3,27.675)) ;
#13609 = CARTESIAN_POINT('',(-72.8,-52.3,27.75)) ;
#13610 = CARTESIAN_POINT('',(-72.875,-52.3,27.675)) ;
#13611 = CARTESIAN_POINT('Origin',(-71.75,-52.3,27.75)) ;
#13612 = CARTESIAN_POINT('Origin',(-71.75,-52.3,27.6)) ;
#13613 = CARTESIAN_POINT('',(-72.8,-52.3,33.4)) ;
#13614 = CARTESIAN_POINT('',(-72.8,-52.3,27.6)) ;
#13615 = CARTESIAN_POINT('Origin',(-71.75,-52.3,33.4)) ;
#13616 = CARTESIAN_POINT('Origin',(-84.75,-52.3,33.4)) ;
#13617 = CARTESIAN_POINT('',(-84.75,-52.3,34.0309036499789)) ;
#13618 = CARTESIAN_POINT('',(-85.8,-52.3,33.4)) ;
#13619 = CARTESIAN_POINT('Origin',(-71.75,-52.3,33.4)) ;
#13620 = CARTESIAN_POINT('',(-71.75,-52.3,34.0309036499789)) ;
#13621 = CARTESIAN_POINT('',(-72.8,-52.3,33.4)) ;
#13622 = CARTESIAN_POINT('Origin',(-84.75,52.3,33.4)) ;
#13623 = CARTESIAN_POINT('',(-84.75,52.3,34.0309036499789)) ;
#13624 = CARTESIAN_POINT('',(-85.8,52.3,33.4)) ;
#13625 = CARTESIAN_POINT('Origin',(-71.75,52.3,33.4)) ;
#13626 = CARTESIAN_POINT('',(-71.75,52.3,34.0309036499789)) ;
#13627 = CARTESIAN_POINT('',(-72.8,52.3,33.4)) ;
#13628 = CARTESIAN_POINT('Origin',(71.75,-52.3,33.4)) ;
#13629 = CARTESIAN_POINT('Ctrl Pts',(70.7183994382024,-52.4957045755694,33.4)) ;
#13630 = CARTESIAN_POINT('Ctrl Pts',(70.7130431211426,-52.4291601614903,33.4042904118456)) ;
#13631 = CARTESIAN_POINT('Ctrl Pts',(70.7105358550768,-52.3635187345962,33.4063305804034)) ;
#13632 = CARTESIAN_POINT('Ctrl Pts',(70.7105358550768,-52.3,33.4063305804034)) ;
#13633 = CARTESIAN_POINT('Ctrl Pts',(70.7105358550768,-52.2364812654038,33.4063305804034)) ;
#13634 = CARTESIAN_POINT('Ctrl Pts',(70.7130431211426,-52.1708398385097,33.4042904118456)) ;
#13635 = CARTESIAN_POINT('Ctrl Pts',(70.7183994382024,-52.1042954244305,33.4)) ;
#13636 = CARTESIAN_POINT('Origin',(72.,-56.3,35.)) ;
#13637 = CARTESIAN_POINT('',(69.95,-55.3,35.)) ;
#13638 = CARTESIAN_POINT('Origin',(72.,-55.3,35.)) ;
#13639 = CARTESIAN_POINT('',(69.95,-49.3,35.)) ;
#13640 = CARTESIAN_POINT('',(69.95,-56.3,35.)) ;
#13641 = CARTESIAN_POINT('Origin',(72.,-49.3,35.)) ;
#13642 = CARTESIAN_POINT('Origin',(84.75,-52.3,33.4)) ;
#13643 = CARTESIAN_POINT('',(84.75,-52.3,34.0309036499789)) ;
#13644 = CARTESIAN_POINT('',(83.7,-52.3,33.4)) ;
#13645 = CARTESIAN_POINT('Origin',(71.75,52.3,33.4)) ;
#13646 = CARTESIAN_POINT('Ctrl Pts',(70.7183994382024,52.1042954244305,33.4)) ;
#13647 = CARTESIAN_POINT('Ctrl Pts',(70.7130431211426,52.1708398385097,33.4042904118456)) ;
#13648 = CARTESIAN_POINT('Ctrl Pts',(70.7105358550768,52.2364812654038,33.4063305804034)) ;
#13649 = CARTESIAN_POINT('Ctrl Pts',(70.7105358550768,52.3,33.4063305804034)) ;
#13650 = CARTESIAN_POINT('Ctrl Pts',(70.7105358550768,52.3635187345962,33.4063305804034)) ;
#13651 = CARTESIAN_POINT('Ctrl Pts',(70.7130431211426,52.4291601614903,33.4042904118456)) ;
#13652 = CARTESIAN_POINT('Ctrl Pts',(70.7183994382024,52.4957045755694,33.4)) ;
#13653 = CARTESIAN_POINT('Origin',(72.,-56.3,35.)) ;
#13654 = CARTESIAN_POINT('',(69.95,49.3,35.)) ;
#13655 = CARTESIAN_POINT('Origin',(72.,49.3,35.)) ;
#13656 = CARTESIAN_POINT('',(69.95,55.3,35.)) ;
#13657 = CARTESIAN_POINT('',(69.95,-56.3,35.)) ;
#13658 = CARTESIAN_POINT('Origin',(72.,55.3,35.)) ;
#13659 = CARTESIAN_POINT('Origin',(84.75,52.3,33.4)) ;
#13660 = CARTESIAN_POINT('',(84.75,52.3,34.0309036499789)) ;
#13661 = CARTESIAN_POINT('',(83.7,52.3,33.4)) ;
#13662 = CARTESIAN_POINT('Origin',(88.75,-45.,50.)) ;
#13663 = CARTESIAN_POINT('',(88.0811225508981,-46.15,50.)) ;
#13664 = CARTESIAN_POINT('',(88.25,-45.,51.15)) ;
#13665 = CARTESIAN_POINT('Ctrl Pts',(88.0811225508981,-46.15,50.)) ;
#13666 = CARTESIAN_POINT('Ctrl Pts',(88.0811225508981,-46.15,50.1453034266508)) ;
#13667 = CARTESIAN_POINT('Ctrl Pts',(88.0902531665979,-46.1207924457676,50.2996897552291)) ;
#13668 = CARTESIAN_POINT('Ctrl Pts',(88.1226395702438,-46.0031862805799,50.5827581865916)) ;
#13669 = CARTESIAN_POINT('Ctrl Pts',(88.1453650465612,-45.9148280935687,50.7115175031603)) ;
#13670 = CARTESIAN_POINT('Ctrl Pts',(88.1875729412465,-45.7115428603744,50.9148027363547)) ;
#13671 = CARTESIAN_POINT('Ctrl Pts',(88.2098812441699,-45.5827731705935,51.0031805967208)) ;
#13672 = CARTESIAN_POINT('Ctrl Pts',(88.2413009851215,-45.2996672843957,51.1208012401597)) ;
#13673 = CARTESIAN_POINT('Ctrl Pts',(88.25,-45.1452671817106,51.15)) ;
#13674 = CARTESIAN_POINT('Ctrl Pts',(88.25,-45.,51.15)) ;
#13675 = CARTESIAN_POINT('Ctrl Pts',(88.25,-45.,51.15)) ;
#13676 = CARTESIAN_POINT('Ctrl Pts',(88.25,-44.8547328182893,51.15)) ;
#13677 = CARTESIAN_POINT('Ctrl Pts',(88.2413009851215,-44.7003327156043,51.1208012401597)) ;
#13678 = CARTESIAN_POINT('Ctrl Pts',(88.2098812441699,-44.4172268294065,51.0031805967208)) ;
#13679 = CARTESIAN_POINT('Ctrl Pts',(88.1875729412465,-44.2884571396256,50.9148027363547)) ;
#13680 = CARTESIAN_POINT('Ctrl Pts',(88.1453650465612,-44.0851719064313,50.7115175031603)) ;
#13681 = CARTESIAN_POINT('Ctrl Pts',(88.1226395702438,-43.9968137194201,50.5827581865916)) ;
#13682 = CARTESIAN_POINT('Ctrl Pts',(88.0902531665979,-43.8792075542324,50.2996897552291)) ;
#13683 = CARTESIAN_POINT('Ctrl Pts',(88.0811225508981,-43.85,50.1453034266508)) ;
#13684 = CARTESIAN_POINT('Ctrl Pts',(88.0811225508981,-43.85,49.8546965733492)) ;
#13685 = CARTESIAN_POINT('Ctrl Pts',(88.0902531665979,-43.8792075542324,49.7003102447709)) ;
#13686 = CARTESIAN_POINT('Ctrl Pts',(88.1226395702438,-43.9968137194201,49.4172418134084)) ;
#13687 = CARTESIAN_POINT('Ctrl Pts',(88.1453650465612,-44.0851719064313,49.2884824968397)) ;
#13688 = CARTESIAN_POINT('Ctrl Pts',(88.1875729412465,-44.2884571396256,49.0851972636453)) ;
#13689 = CARTESIAN_POINT('Ctrl Pts',(88.2098812441699,-44.4172268294065,48.9968194032792)) ;
#13690 = CARTESIAN_POINT('Ctrl Pts',(88.2413009851215,-44.7003327156043,48.8791987598403)) ;
#13691 = CARTESIAN_POINT('Ctrl Pts',(88.25,-44.8547328182894,48.85)) ;
#13692 = CARTESIAN_POINT('Ctrl Pts',(88.25,-45.1452671817106,48.85)) ;
#13693 = CARTESIAN_POINT('Ctrl Pts',(88.2413009851215,-45.2996672843957,48.8791987598403)) ;
#13694 = CARTESIAN_POINT('Ctrl Pts',(88.2098812441699,-45.5827731705935,48.9968194032792)) ;
#13695 = CARTESIAN_POINT('Ctrl Pts',(88.1875729412465,-45.7115428603744,49.0851972636453)) ;
#13696 = CARTESIAN_POINT('Ctrl Pts',(88.1453650465612,-45.9148280935687,49.2884824968397)) ;
#13697 = CARTESIAN_POINT('Ctrl Pts',(88.1226395702438,-46.0031862805799,49.4172418134084)) ;
#13698 = CARTESIAN_POINT('Ctrl Pts',(88.0902531665979,-46.1207924457676,49.7003102447709)) ;
#13699 = CARTESIAN_POINT('Ctrl Pts',(88.0811225508981,-46.15,49.8546965733492)) ;
#13700 = CARTESIAN_POINT('Ctrl Pts',(88.0811225508981,-46.15,50.)) ;
#13701 = CARTESIAN_POINT('',(87.2,-45.,51.15)) ;
#13702 = CARTESIAN_POINT('',(88.75,-45.,51.15)) ;
#13703 = CARTESIAN_POINT('',(86.9666155414412,-43.85,50.)) ;
#13704 = CARTESIAN_POINT('Ctrl Pts',(86.9666155414412,-43.85,50.)) ;
#13705 = CARTESIAN_POINT('Ctrl Pts',(86.9666155414412,-43.85,50.1461583267558)) ;
#13706 = CARTESIAN_POINT('Ctrl Pts',(86.9796573686722,-43.8795285636834,50.3008398252782)) ;
#13707 = CARTESIAN_POINT('Ctrl Pts',(87.0250928731078,-43.9973311263918,50.5836234155483)) ;
#13708 = CARTESIAN_POINT('Ctrl Pts',(87.0566642086003,-44.0855389722715,50.7118845690005)) ;
#13709 = CARTESIAN_POINT('Ctrl Pts',(87.1147290825117,-44.2880237720613,50.9143693687904)) ;
#13710 = CARTESIAN_POINT('Ctrl Pts',(87.1452181894816,-44.4163199277569,51.0026469087132)) ;
#13711 = CARTESIAN_POINT('Ctrl Pts',(87.188113941166,-44.6992388624653,51.1205025788281)) ;
#13712 = CARTESIAN_POINT('Ctrl Pts',(87.2,-44.8539739365597,51.15)) ;
#13713 = CARTESIAN_POINT('Ctrl Pts',(87.2,-45.,51.15)) ;
#13714 = CARTESIAN_POINT('Ctrl Pts',(87.2,-45.,51.15)) ;
#13715 = CARTESIAN_POINT('Ctrl Pts',(87.2,-45.1460260634403,51.15)) ;
#13716 = CARTESIAN_POINT('Ctrl Pts',(87.188113941166,-45.3007611375347,51.1205025788281)) ;
#13717 = CARTESIAN_POINT('Ctrl Pts',(87.1452181894816,-45.5836800722431,51.0026469087132)) ;
#13718 = CARTESIAN_POINT('Ctrl Pts',(87.1147290825117,-45.7119762279387,50.9143693687904)) ;
#13719 = CARTESIAN_POINT('Ctrl Pts',(87.0566642086003,-45.9144610277285,50.7118845690005)) ;
#13720 = CARTESIAN_POINT('Ctrl Pts',(87.0250928731078,-46.0026688736082,50.5836234155483)) ;
#13721 = CARTESIAN_POINT('Ctrl Pts',(86.9796573686722,-46.1204714363166,50.3008398252782)) ;
#13722 = CARTESIAN_POINT('Ctrl Pts',(86.9666155414412,-46.15,50.1461583267558)) ;
#13723 = CARTESIAN_POINT('Ctrl Pts',(86.9666155414412,-46.15,49.8538416732442)) ;
#13724 = CARTESIAN_POINT('Ctrl Pts',(86.9796573686722,-46.1204714363166,49.6991601747218)) ;
#13725 = CARTESIAN_POINT('Ctrl Pts',(87.0250928731078,-46.0026688736082,49.4163765844517)) ;
#13726 = CARTESIAN_POINT('Ctrl Pts',(87.0566642086003,-45.9144610277285,49.2881154309995)) ;
#13727 = CARTESIAN_POINT('Ctrl Pts',(87.1147290825117,-45.7119762279387,49.0856306312096)) ;
#13728 = CARTESIAN_POINT('Ctrl Pts',(87.1452181894816,-45.5836800722431,48.9973530912868)) ;
#13729 = CARTESIAN_POINT('Ctrl Pts',(87.188113941166,-45.3007611375347,48.8794974211719)) ;
#13730 = CARTESIAN_POINT('Ctrl Pts',(87.2,-45.1460260634403,48.85)) ;
#13731 = CARTESIAN_POINT('Ctrl Pts',(87.2,-44.8539739365597,48.85)) ;
#13732 = CARTESIAN_POINT('Ctrl Pts',(87.188113941166,-44.6992388624653,48.8794974211719)) ;
#13733 = CARTESIAN_POINT('Ctrl Pts',(87.1452181894816,-44.4163199277569,48.9973530912868)) ;
#13734 = CARTESIAN_POINT('Ctrl Pts',(87.1147290825117,-44.2880237720613,49.0856306312096)) ;
#13735 = CARTESIAN_POINT('Ctrl Pts',(87.0566642086003,-44.0855389722715,49.2881154309995)) ;
#13736 = CARTESIAN_POINT('Ctrl Pts',(87.0250928731078,-43.9973311263918,49.4163765844517)) ;
#13737 = CARTESIAN_POINT('Ctrl Pts',(86.9796573686722,-43.8795285636834,49.6991601747218)) ;
#13738 = CARTESIAN_POINT('Ctrl Pts',(86.9666155414412,-43.85,49.8538416732443)) ;
#13739 = CARTESIAN_POINT('Ctrl Pts',(86.9666155414412,-43.85,50.)) ;
#13740 = CARTESIAN_POINT('Origin',(84.25,-45.,55.)) ;
#13741 = CARTESIAN_POINT('',(81.3,-45.,55.)) ;
#13742 = CARTESIAN_POINT('Origin',(84.25,-45.,55.)) ;
#13743 = CARTESIAN_POINT('',(81.3,-45.,41.)) ;
#13744 = CARTESIAN_POINT('',(81.3,-45.,55.)) ;
#13745 = CARTESIAN_POINT('Origin',(84.25,-45.,41.)) ;
#13746 = CARTESIAN_POINT('Origin',(84.25,-45.,41.)) ;
#13747 = CARTESIAN_POINT('Origin',(88.75,45.,50.)) ;
#13748 = CARTESIAN_POINT('',(88.0811225508981,43.85,50.)) ;
#13749 = CARTESIAN_POINT('',(88.25,45.,51.15)) ;
#13750 = CARTESIAN_POINT('Ctrl Pts',(88.0811225508981,43.85,50.)) ;
#13751 = CARTESIAN_POINT('Ctrl Pts',(88.0811225508981,43.85,50.1453034266508)) ;
#13752 = CARTESIAN_POINT('Ctrl Pts',(88.0902531665979,43.8792075542324,50.2996897552291)) ;
#13753 = CARTESIAN_POINT('Ctrl Pts',(88.1226395702438,43.9968137194201,50.5827581865916)) ;
#13754 = CARTESIAN_POINT('Ctrl Pts',(88.1453650465612,44.0851719064313,50.7115175031603)) ;
#13755 = CARTESIAN_POINT('Ctrl Pts',(88.1875729412465,44.2884571396256,50.9148027363547)) ;
#13756 = CARTESIAN_POINT('Ctrl Pts',(88.2098812441699,44.4172268294065,51.0031805967208)) ;
#13757 = CARTESIAN_POINT('Ctrl Pts',(88.2413009851215,44.7003327156042,51.1208012401597)) ;
#13758 = CARTESIAN_POINT('Ctrl Pts',(88.25,44.8547328182894,51.15)) ;
#13759 = CARTESIAN_POINT('Ctrl Pts',(88.25,45.,51.15)) ;
#13760 = CARTESIAN_POINT('Ctrl Pts',(88.25,45.,51.15)) ;
#13761 = CARTESIAN_POINT('Ctrl Pts',(88.25,45.1452671817106,51.15)) ;
#13762 = CARTESIAN_POINT('Ctrl Pts',(88.2413009851215,45.2996672843957,51.1208012401597)) ;
#13763 = CARTESIAN_POINT('Ctrl Pts',(88.2098812441699,45.5827731705935,51.0031805967208)) ;
#13764 = CARTESIAN_POINT('Ctrl Pts',(88.1875729412465,45.7115428603744,50.9148027363547)) ;
#13765 = CARTESIAN_POINT('Ctrl Pts',(88.1453650465612,45.9148280935687,50.7115175031603)) ;
#13766 = CARTESIAN_POINT('Ctrl Pts',(88.1226395702438,46.0031862805799,50.5827581865916)) ;
#13767 = CARTESIAN_POINT('Ctrl Pts',(88.0902531665979,46.1207924457676,50.2996897552291)) ;
#13768 = CARTESIAN_POINT('Ctrl Pts',(88.0811225508981,46.15,50.1453034266508)) ;
#13769 = CARTESIAN_POINT('Ctrl Pts',(88.0811225508981,46.15,49.8546965733492)) ;
#13770 = CARTESIAN_POINT('Ctrl Pts',(88.0902531665979,46.1207924457676,49.7003102447709)) ;
#13771 = CARTESIAN_POINT('Ctrl Pts',(88.1226395702438,46.0031862805799,49.4172418134084)) ;
#13772 = CARTESIAN_POINT('Ctrl Pts',(88.1453650465612,45.9148280935687,49.2884824968397)) ;
#13773 = CARTESIAN_POINT('Ctrl Pts',(88.1875729412465,45.7115428603744,49.0851972636453)) ;
#13774 = CARTESIAN_POINT('Ctrl Pts',(88.2098812441699,45.5827731705935,48.9968194032792)) ;
#13775 = CARTESIAN_POINT('Ctrl Pts',(88.2413009851215,45.2996672843957,48.8791987598403)) ;
#13776 = CARTESIAN_POINT('Ctrl Pts',(88.25,45.1452671817106,48.85)) ;
#13777 = CARTESIAN_POINT('Ctrl Pts',(88.25,44.8547328182894,48.85)) ;
#13778 = CARTESIAN_POINT('Ctrl Pts',(88.2413009851215,44.7003327156043,48.8791987598403)) ;
#13779 = CARTESIAN_POINT('Ctrl Pts',(88.2098812441699,44.4172268294065,48.9968194032792)) ;
#13780 = CARTESIAN_POINT('Ctrl Pts',(88.1875729412465,44.2884571396256,49.0851972636453)) ;
#13781 = CARTESIAN_POINT('Ctrl Pts',(88.1453650465612,44.0851719064313,49.2884824968397)) ;
#13782 = CARTESIAN_POINT('Ctrl Pts',(88.1226395702438,43.9968137194201,49.4172418134084)) ;
#13783 = CARTESIAN_POINT('Ctrl Pts',(88.0902531665979,43.8792075542324,49.7003102447709)) ;
#13784 = CARTESIAN_POINT('Ctrl Pts',(88.0811225508981,43.85,49.8546965733492)) ;
#13785 = CARTESIAN_POINT('Ctrl Pts',(88.0811225508981,43.85,50.)) ;
#13786 = CARTESIAN_POINT('',(87.2,45.,51.15)) ;
#13787 = CARTESIAN_POINT('',(88.75,45.,51.15)) ;
#13788 = CARTESIAN_POINT('',(86.9666155414412,46.15,50.)) ;
#13789 = CARTESIAN_POINT('Ctrl Pts',(86.9666155414412,46.15,50.)) ;
#13790 = CARTESIAN_POINT('Ctrl Pts',(86.9666155414412,46.15,50.1461583267558)) ;
#13791 = CARTESIAN_POINT('Ctrl Pts',(86.9796573686722,46.1204714363166,50.3008398252782)) ;
#13792 = CARTESIAN_POINT('Ctrl Pts',(87.0250928731078,46.0026688736082,50.5836234155483)) ;
#13793 = CARTESIAN_POINT('Ctrl Pts',(87.0566642086003,45.9144610277285,50.7118845690005)) ;
#13794 = CARTESIAN_POINT('Ctrl Pts',(87.1147290825117,45.7119762279387,50.9143693687904)) ;
#13795 = CARTESIAN_POINT('Ctrl Pts',(87.1452181894816,45.5836800722431,51.0026469087132)) ;
#13796 = CARTESIAN_POINT('Ctrl Pts',(87.188113941166,45.3007611375347,51.1205025788281)) ;
#13797 = CARTESIAN_POINT('Ctrl Pts',(87.2,45.1460260634403,51.15)) ;
#13798 = CARTESIAN_POINT('Ctrl Pts',(87.2,45.,51.15)) ;
#13799 = CARTESIAN_POINT('Ctrl Pts',(87.2,45.,51.15)) ;
#13800 = CARTESIAN_POINT('Ctrl Pts',(87.2,44.8539739365597,51.15)) ;
#13801 = CARTESIAN_POINT('Ctrl Pts',(87.188113941166,44.6992388624653,51.1205025788281)) ;
#13802 = CARTESIAN_POINT('Ctrl Pts',(87.1452181894816,44.4163199277569,51.0026469087132)) ;
#13803 = CARTESIAN_POINT('Ctrl Pts',(87.1147290825117,44.2880237720613,50.9143693687904)) ;
#13804 = CARTESIAN_POINT('Ctrl Pts',(87.0566642086003,44.0855389722715,50.7118845690005)) ;
#13805 = CARTESIAN_POINT('Ctrl Pts',(87.0250928731078,43.9973311263918,50.5836234155483)) ;
#13806 = CARTESIAN_POINT('Ctrl Pts',(86.9796573686722,43.8795285636834,50.3008398252782)) ;
#13807 = CARTESIAN_POINT('Ctrl Pts',(86.9666155414412,43.85,50.1461583267558)) ;
#13808 = CARTESIAN_POINT('Ctrl Pts',(86.9666155414412,43.85,49.8538416732442)) ;
#13809 = CARTESIAN_POINT('Ctrl Pts',(86.9796573686722,43.8795285636834,49.6991601747218)) ;
#13810 = CARTESIAN_POINT('Ctrl Pts',(87.0250928731078,43.9973311263918,49.4163765844517)) ;
#13811 = CARTESIAN_POINT('Ctrl Pts',(87.0566642086003,44.0855389722715,49.2881154309995)) ;
#13812 = CARTESIAN_POINT('Ctrl Pts',(87.1147290825117,44.2880237720613,49.0856306312096)) ;
#13813 = CARTESIAN_POINT('Ctrl Pts',(87.1452181894816,44.4163199277569,48.9973530912868)) ;
#13814 = CARTESIAN_POINT('Ctrl Pts',(87.188113941166,44.6992388624653,48.8794974211719)) ;
#13815 = CARTESIAN_POINT('Ctrl Pts',(87.2,44.8539739365597,48.85)) ;
#13816 = CARTESIAN_POINT('Ctrl Pts',(87.2,45.1460260634403,48.85)) ;
#13817 = CARTESIAN_POINT('Ctrl Pts',(87.188113941166,45.3007611375347,48.8794974211719)) ;
#13818 = CARTESIAN_POINT('Ctrl Pts',(87.1452181894816,45.5836800722431,48.9973530912868)) ;
#13819 = CARTESIAN_POINT('Ctrl Pts',(87.1147290825117,45.7119762279387,49.0856306312096)) ;
#13820 = CARTESIAN_POINT('Ctrl Pts',(87.0566642086003,45.9144610277285,49.2881154309995)) ;
#13821 = CARTESIAN_POINT('Ctrl Pts',(87.0250928731078,46.0026688736082,49.4163765844517)) ;
#13822 = CARTESIAN_POINT('Ctrl Pts',(86.9796573686722,46.1204714363166,49.6991601747218)) ;
#13823 = CARTESIAN_POINT('Ctrl Pts',(86.9666155414412,46.15,49.8538416732442)) ;
#13824 = CARTESIAN_POINT('Ctrl Pts',(86.9666155414412,46.15,50.)) ;
#13825 = CARTESIAN_POINT('Origin',(84.25,45.,55.)) ;
#13826 = CARTESIAN_POINT('',(81.3,45.,55.)) ;
#13827 = CARTESIAN_POINT('Origin',(84.25,45.,55.)) ;
#13828 = CARTESIAN_POINT('',(81.3,45.,41.)) ;
#13829 = CARTESIAN_POINT('',(81.3,45.,55.)) ;
#13830 = CARTESIAN_POINT('Origin',(84.25,45.,41.)) ;
#13831 = CARTESIAN_POINT('Origin',(84.25,45.,41.)) ;
#13832 = CARTESIAN_POINT('Origin',(77.,-4.,35.)) ;
#13833 = CARTESIAN_POINT('',(74.95,2.3,35.)) ;
#13834 = CARTESIAN_POINT('Origin',(77.,2.3,35.)) ;
#13835 = CARTESIAN_POINT('',(74.95,3.3,35.)) ;
#13836 = CARTESIAN_POINT('',(74.95,-4.,35.)) ;
#13837 = CARTESIAN_POINT('Origin',(77.,3.3,35.)) ;
#13838 = CARTESIAN_POINT('Origin',(77.,-4.,35.)) ;
#13839 = CARTESIAN_POINT('',(74.95,-3.3,35.)) ;
#13840 = CARTESIAN_POINT('Origin',(77.,-3.3,35.)) ;
#13841 = CARTESIAN_POINT('',(74.95,-2.3,35.)) ;
#13842 = CARTESIAN_POINT('',(74.95,-4.,35.)) ;
#13843 = CARTESIAN_POINT('Origin',(77.,-2.3,35.)) ;
#13844 = CARTESIAN_POINT('Origin',(72.,-56.3,35.)) ;
#13845 = CARTESIAN_POINT('',(73.69525,3.3,36.1526610245428)) ;
#13846 = CARTESIAN_POINT('',(73.69525,2.3,36.1526610245428)) ;
#13847 = CARTESIAN_POINT('',(73.69525,-56.3,36.1526610245428)) ;
#13848 = CARTESIAN_POINT('',(73.5,3.3,33.6026811387518)) ;
#13849 = CARTESIAN_POINT('Origin',(72.,3.3,35.)) ;
#13850 = CARTESIAN_POINT('',(73.5,2.3,33.6026811387518)) ;
#13851 = CARTESIAN_POINT('',(73.5,-56.3,33.6026811387518)) ;
#13852 = CARTESIAN_POINT('Origin',(72.,2.3,35.)) ;
#13853 = CARTESIAN_POINT('Origin',(72.,-56.3,35.)) ;
#13854 = CARTESIAN_POINT('',(73.69525,-2.3,36.1526610245428)) ;
#13855 = CARTESIAN_POINT('',(73.69525,-3.3,36.1526610245428)) ;
#13856 = CARTESIAN_POINT('',(73.69525,-56.3,36.1526610245428)) ;
#13857 = CARTESIAN_POINT('',(73.5,-2.3,33.6026811387518)) ;
#13858 = CARTESIAN_POINT('Origin',(72.,-2.3,35.)) ;
#13859 = CARTESIAN_POINT('',(73.5,-3.3,33.6026811387518)) ;
#13860 = CARTESIAN_POINT('',(73.5,-56.3,33.6026811387518)) ;
#13861 = CARTESIAN_POINT('Origin',(72.,-3.3,35.)) ;
#13862 = CARTESIAN_POINT('Origin',(73.5,-3.3,30.)) ;
#13863 = CARTESIAN_POINT('',(73.5,-2.3,30.)) ;
#13864 = CARTESIAN_POINT('',(73.5,-2.3,30.)) ;
#13865 = CARTESIAN_POINT('',(73.5,-3.3,30.)) ;
#13866 = CARTESIAN_POINT('',(73.5,-3.3,30.)) ;
#13867 = CARTESIAN_POINT('',(73.5,-3.3,30.)) ;
#13868 = CARTESIAN_POINT('Origin',(77.375,-2.3,34.25)) ;
#13869 = CARTESIAN_POINT('',(80.5,-2.3,35.)) ;
#13870 = CARTESIAN_POINT('Origin',(77.,-2.3,35.)) ;
#13871 = CARTESIAN_POINT('',(81.25,-2.3,35.)) ;
#13872 = CARTESIAN_POINT('',(80.5,-2.3,35.)) ;
#13873 = CARTESIAN_POINT('',(81.25,-2.3,30.)) ;
#13874 = CARTESIAN_POINT('',(81.25,-2.3,31.675)) ;
#13875 = CARTESIAN_POINT('',(81.25,-2.3,30.)) ;
#13876 = CARTESIAN_POINT('Origin',(73.5,2.3,30.)) ;
#13877 = CARTESIAN_POINT('',(73.5,3.3,30.)) ;
#13878 = CARTESIAN_POINT('',(73.5,3.3,30.)) ;
#13879 = CARTESIAN_POINT('',(73.5,2.3,30.)) ;
#13880 = CARTESIAN_POINT('',(73.5,2.3,30.)) ;
#13881 = CARTESIAN_POINT('',(73.5,2.3,30.)) ;
#13882 = CARTESIAN_POINT('Origin',(77.375,3.3,34.25)) ;
#13883 = CARTESIAN_POINT('',(80.5,3.3,35.)) ;
#13884 = CARTESIAN_POINT('Origin',(77.,3.3,35.)) ;
#13885 = CARTESIAN_POINT('',(81.25,3.3,35.)) ;
#13886 = CARTESIAN_POINT('',(80.5,3.3,35.)) ;
#13887 = CARTESIAN_POINT('',(81.25,3.3,30.)) ;
#13888 = CARTESIAN_POINT('',(81.25,3.3,31.675)) ;
#13889 = CARTESIAN_POINT('',(81.25,3.3,30.)) ;
#13890 = CARTESIAN_POINT('Origin',(43.625,55.05,38.85)) ;
#13891 = CARTESIAN_POINT('',(-87.25,55.3,38.6)) ;
#13892 = CARTESIAN_POINT('',(-87.25,54.8,39.1)) ;
#13893 = CARTESIAN_POINT('',(-87.25,57.55,36.35)) ;
#13894 = CARTESIAN_POINT('',(87.25,54.8,39.1)) ;
#13895 = CARTESIAN_POINT('',(43.625,54.8,39.1)) ;
#13896 = CARTESIAN_POINT('',(87.25,55.3,38.6)) ;
#13897 = CARTESIAN_POINT('',(87.25,56.05,37.85)) ;
#13898 = CARTESIAN_POINT('',(43.625,55.3,38.6)) ;
#13899 = CARTESIAN_POINT('Origin',(87.25,55.3,29.1)) ;
#13900 = CARTESIAN_POINT('',(87.25,55.3,29.1)) ;
#13901 = CARTESIAN_POINT('',(87.25,55.3,29.1)) ;
#13902 = CARTESIAN_POINT('',(69.25,55.3,29.1)) ;
#13903 = CARTESIAN_POINT('',(87.25,55.3,29.1)) ;
#13904 = CARTESIAN_POINT('',(-69.25,55.3,29.1)) ;
#13905 = CARTESIAN_POINT('',(87.25,55.3,29.1)) ;
#13906 = CARTESIAN_POINT('',(-87.25,55.3,29.1)) ;
#13907 = CARTESIAN_POINT('',(87.25,55.3,29.1)) ;
#13908 = CARTESIAN_POINT('',(-87.25,55.3,29.1)) ;
#13909 = CARTESIAN_POINT('Origin',(87.25,49.3,29.1)) ;
#13910 = CARTESIAN_POINT('',(87.25,47.6457513110646,39.1)) ;
#13911 = CARTESIAN_POINT('',(87.25,-55.3,39.1)) ;
#13912 = CARTESIAN_POINT('',(87.25,47.6457513110646,38.6)) ;
#13913 = CARTESIAN_POINT('',(87.25,47.6457513110646,46.8)) ;
#13914 = CARTESIAN_POINT('',(87.25,42.3542486889354,38.6)) ;
#13915 = CARTESIAN_POINT('',(87.25,47.15,38.6)) ;
#13916 = CARTESIAN_POINT('',(87.25,42.3542486889354,39.1)) ;
#13917 = CARTESIAN_POINT('',(87.25,42.3542486889354,46.8)) ;
#13918 = CARTESIAN_POINT('',(87.25,-42.3542486889354,39.1)) ;
#13919 = CARTESIAN_POINT('',(87.25,-55.3,39.1)) ;
#13920 = CARTESIAN_POINT('',(87.25,-42.3542486889354,38.6)) ;
#13921 = CARTESIAN_POINT('',(87.25,-42.3542486889354,46.8)) ;
#13922 = CARTESIAN_POINT('',(87.25,-47.6457513110646,38.6)) ;
#13923 = CARTESIAN_POINT('',(87.25,2.15,38.6)) ;
#13924 = CARTESIAN_POINT('',(87.25,-47.6457513110646,39.1)) ;
#13925 = CARTESIAN_POINT('',(87.25,-47.6457513110646,46.8)) ;
#13926 = CARTESIAN_POINT('',(87.25,-54.8,39.1)) ;
#13927 = CARTESIAN_POINT('',(87.25,-55.3,39.1)) ;
#13928 = CARTESIAN_POINT('',(87.25,-55.3,38.6)) ;
#13929 = CARTESIAN_POINT('',(87.25,-31.4,62.5)) ;
#13930 = CARTESIAN_POINT('',(87.25,-55.3,29.1)) ;
#13931 = CARTESIAN_POINT('',(87.25,-55.3,29.1)) ;
#13932 = CARTESIAN_POINT('',(87.25,-59.3,29.1)) ;
#13933 = CARTESIAN_POINT('',(87.25,-59.3,29.1)) ;
#13934 = CARTESIAN_POINT('',(87.25,-59.3,27.6)) ;
#13935 = CARTESIAN_POINT('',(87.25,-45.3,29.1)) ;
#13936 = CARTESIAN_POINT('',(87.25,-45.3,27.6)) ;
#13937 = CARTESIAN_POINT('',(87.25,45.3,29.1)) ;
#13938 = CARTESIAN_POINT('',(87.25,-55.3,29.1)) ;
#13939 = CARTESIAN_POINT('',(87.25,45.3,27.6)) ;
#13940 = CARTESIAN_POINT('',(87.25,59.3,29.1)) ;
#13941 = CARTESIAN_POINT('',(87.25,59.3,27.6)) ;
#13942 = CARTESIAN_POINT('',(87.25,45.3,29.1)) ;
#13943 = CARTESIAN_POINT('Origin',(-43.625,-55.05,38.85)) ;
#13944 = CARTESIAN_POINT('',(-87.25,-54.8,39.1)) ;
#13945 = CARTESIAN_POINT('',(-43.625,-54.8,39.1)) ;
#13946 = CARTESIAN_POINT('',(-87.25,-55.3,38.6)) ;
#13947 = CARTESIAN_POINT('',(-87.25,-29.9,64.)) ;
#13948 = CARTESIAN_POINT('',(-43.625,-55.3,38.6)) ;
#13949 = CARTESIAN_POINT('Origin',(-87.25,-55.3,29.1)) ;
#13950 = CARTESIAN_POINT('',(-87.25,-55.3,29.1)) ;
#13951 = CARTESIAN_POINT('',(-87.25,-55.3,29.1)) ;
#13952 = CARTESIAN_POINT('',(-69.25,-55.3,29.1)) ;
#13953 = CARTESIAN_POINT('',(-87.25,-55.3,29.1)) ;
#13954 = CARTESIAN_POINT('',(69.25,-55.3,29.1)) ;
#13955 = CARTESIAN_POINT('',(-87.25,-55.3,29.1)) ;
#13956 = CARTESIAN_POINT('',(-87.25,-55.3,29.1)) ;
#13957 = CARTESIAN_POINT('Origin',(84.25,-45.,46.8)) ;
#13958 = CARTESIAN_POINT('',(80.25,-45.,55.)) ;
#13959 = CARTESIAN_POINT('Origin',(84.25,-45.,55.)) ;
#13960 = CARTESIAN_POINT('',(80.25,-45.,38.6)) ;
#13961 = CARTESIAN_POINT('',(80.25,-45.,46.8)) ;
#13962 = CARTESIAN_POINT('',(81.25,-47.6457513110646,38.6)) ;
#13963 = CARTESIAN_POINT('Origin',(84.25,-45.,38.6)) ;
#13964 = CARTESIAN_POINT('',(81.25,-47.6457513110646,39.1)) ;
#13965 = CARTESIAN_POINT('',(81.25,-47.6457513110646,46.8)) ;
#13966 = CARTESIAN_POINT('Origin',(84.25,-45.,39.1)) ;
#13967 = CARTESIAN_POINT('Origin',(84.25,-45.,38.6)) ;
#13968 = CARTESIAN_POINT('',(81.25,-42.3542486889354,39.1)) ;
#13969 = CARTESIAN_POINT('Origin',(84.25,-45.,39.1)) ;
#13970 = CARTESIAN_POINT('',(81.25,-42.3542486889354,38.6)) ;
#13971 = CARTESIAN_POINT('',(81.25,-42.3542486889354,46.8)) ;
#13972 = CARTESIAN_POINT('Origin',(84.25,-45.,38.6)) ;
#13973 = CARTESIAN_POINT('Origin',(88.25,-45.,38.6)) ;
#13974 = CARTESIAN_POINT('Origin',(88.25,-45.,38.6)) ;
#13975 = CARTESIAN_POINT('',(81.25,2.15,38.6)) ;
#13976 = CARTESIAN_POINT('Origin',(84.25,-45.,55.)) ;
#13977 = CARTESIAN_POINT('Origin',(81.25,49.3,29.1)) ;
#13978 = CARTESIAN_POINT('',(81.25,42.3542486889354,39.1)) ;
#13979 = CARTESIAN_POINT('',(81.25,49.3,39.1)) ;
#13980 = CARTESIAN_POINT('',(81.25,42.3542486889354,38.6)) ;
#13981 = CARTESIAN_POINT('',(81.25,42.3542486889354,46.8)) ;
#13982 = CARTESIAN_POINT('',(81.25,47.6457513110646,38.6)) ;
#13983 = CARTESIAN_POINT('',(81.25,47.15,38.6)) ;
#13984 = CARTESIAN_POINT('',(81.25,47.6457513110646,39.1)) ;
#13985 = CARTESIAN_POINT('',(81.25,47.6457513110646,46.8)) ;
#13986 = CARTESIAN_POINT('',(81.25,49.3,39.1)) ;
#13987 = CARTESIAN_POINT('',(81.25,49.3,39.1)) ;
#13988 = CARTESIAN_POINT('',(81.25,49.3,29.1)) ;
#13989 = CARTESIAN_POINT('',(81.25,49.3,29.1)) ;
#13990 = CARTESIAN_POINT('',(81.25,45.3,29.1)) ;
#13991 = CARTESIAN_POINT('',(81.25,49.3,29.1)) ;
#13992 = CARTESIAN_POINT('',(81.25,-45.3,29.1)) ;
#13993 = CARTESIAN_POINT('',(81.25,49.3,29.1)) ;
#13994 = CARTESIAN_POINT('',(81.25,-49.3,29.1)) ;
#13995 = CARTESIAN_POINT('',(81.25,49.3,29.1)) ;
#13996 = CARTESIAN_POINT('',(81.25,-49.3,39.1)) ;
#13997 = CARTESIAN_POINT('',(81.25,-49.3,29.1)) ;
#13998 = CARTESIAN_POINT('',(81.25,49.3,39.1)) ;
#13999 = CARTESIAN_POINT('',(81.25,2.3,35.)) ;
#14000 = CARTESIAN_POINT('',(81.25,25.8,35.)) ;
#14001 = CARTESIAN_POINT('',(81.25,2.3,30.)) ;
#14002 = CARTESIAN_POINT('',(81.25,2.3,31.675)) ;
#14003 = CARTESIAN_POINT('',(81.25,25.8,30.)) ;
#14004 = CARTESIAN_POINT('',(81.25,-3.3,35.)) ;
#14005 = CARTESIAN_POINT('',(81.25,23.,35.)) ;
#14006 = CARTESIAN_POINT('',(81.25,-3.3,30.)) ;
#14007 = CARTESIAN_POINT('',(81.25,-3.3,31.675)) ;
#14008 = CARTESIAN_POINT('',(81.25,23.,30.)) ;
#14009 = CARTESIAN_POINT('Origin',(0.,52.3,39.1)) ;
#14010 = CARTESIAN_POINT('Origin',(84.25,45.,39.1)) ;
#14011 = CARTESIAN_POINT('Origin',(81.25,-3.3,30.)) ;
#14012 = CARTESIAN_POINT('',(81.25,-3.3,30.)) ;
#14013 = CARTESIAN_POINT('Origin',(80.5,-3.3,35.)) ;
#14014 = CARTESIAN_POINT('',(80.5,-3.3,35.)) ;
#14015 = CARTESIAN_POINT('',(80.5,-3.3,35.)) ;
#14016 = CARTESIAN_POINT('',(80.5,-3.3,35.)) ;
#14017 = CARTESIAN_POINT('Origin',(77.,-3.3,35.)) ;
#14018 = CARTESIAN_POINT('Origin',(77.,-3.3,35.)) ;
#14019 = CARTESIAN_POINT('Origin',(77.375,-3.3,34.25)) ;
#14020 = CARTESIAN_POINT('Origin',(-38.,-43.8,31.)) ;
#14021 = CARTESIAN_POINT('',(-81.25,-49.3,31.)) ;
#14022 = CARTESIAN_POINT('',(-81.25,-38.3,31.)) ;
#14023 = CARTESIAN_POINT('',(-81.25,-46.55,31.)) ;
#14024 = CARTESIAN_POINT('',(6.,-49.3,31.)) ;
#14025 = CARTESIAN_POINT('',(24.625,-49.3,31.)) ;
#14026 = CARTESIAN_POINT('',(6.,-38.3,31.)) ;
#14027 = CARTESIAN_POINT('',(6.,-49.3,31.)) ;
#14028 = CARTESIAN_POINT('',(6.,-38.3,31.)) ;
#14029 = CARTESIAN_POINT('Origin',(6.,-38.3,29.1)) ;
#14030 = CARTESIAN_POINT('',(-81.25,-38.3,29.1)) ;
#14031 = CARTESIAN_POINT('',(-81.25,-38.3,29.1)) ;
#14032 = CARTESIAN_POINT('',(6.,-38.3,29.1)) ;
#14033 = CARTESIAN_POINT('',(6.,-38.3,29.1)) ;
#14034 = CARTESIAN_POINT('',(6.,-38.3,29.1)) ;
#14035 = CARTESIAN_POINT('Origin',(6.,-49.3,29.1)) ;
#14036 = CARTESIAN_POINT('',(6.,-49.3,29.1)) ;
#14037 = CARTESIAN_POINT('',(6.,-49.3,29.1)) ;
#14038 = CARTESIAN_POINT('',(6.,-49.3,29.1)) ;
#14039 = CARTESIAN_POINT('Origin',(84.25,45.,46.8)) ;
#14040 = CARTESIAN_POINT('',(80.25,45.,55.)) ;
#14041 = CARTESIAN_POINT('Origin',(84.25,45.,55.)) ;
#14042 = CARTESIAN_POINT('',(80.25,45.,38.6)) ;
#14043 = CARTESIAN_POINT('',(80.25,45.,46.8)) ;
#14044 = CARTESIAN_POINT('Origin',(84.25,45.,38.6)) ;
#14045 = CARTESIAN_POINT('Origin',(84.25,45.,38.6)) ;
#14046 = CARTESIAN_POINT('Origin',(84.25,45.,39.1)) ;
#14047 = CARTESIAN_POINT('Origin',(84.25,45.,38.6)) ;
#14048 = CARTESIAN_POINT('Origin',(88.25,45.,38.6)) ;
#14049 = CARTESIAN_POINT('Origin',(88.25,45.,38.6)) ;
#14050 = CARTESIAN_POINT('Origin',(84.25,45.,55.)) ;
#14051 = CARTESIAN_POINT('Origin',(81.25,2.3,30.)) ;
#14052 = CARTESIAN_POINT('',(81.25,2.3,30.)) ;
#14053 = CARTESIAN_POINT('Origin',(80.5,2.3,35.)) ;
#14054 = CARTESIAN_POINT('',(80.5,2.3,35.)) ;
#14055 = CARTESIAN_POINT('',(80.5,2.3,35.)) ;
#14056 = CARTESIAN_POINT('',(80.5,2.3,35.)) ;
#14057 = CARTESIAN_POINT('Origin',(77.,2.3,35.)) ;
#14058 = CARTESIAN_POINT('Origin',(77.,2.3,35.)) ;
#14059 = CARTESIAN_POINT('Origin',(77.375,2.3,34.25)) ;
#14060 = CARTESIAN_POINT('Origin',(-38.,43.8,31.)) ;
#14061 = CARTESIAN_POINT('',(-81.25,38.3,31.)) ;
#14062 = CARTESIAN_POINT('',(-81.25,49.3,31.)) ;
#14063 = CARTESIAN_POINT('',(-81.25,-2.75,31.)) ;
#14064 = CARTESIAN_POINT('',(6.,38.3,31.)) ;
#14065 = CARTESIAN_POINT('',(-82.,38.3,31.)) ;
#14066 = CARTESIAN_POINT('',(6.,49.3,31.)) ;
#14067 = CARTESIAN_POINT('',(6.,38.3,31.)) ;
#14068 = CARTESIAN_POINT('',(-62.625,49.3,31.)) ;
#14069 = CARTESIAN_POINT('Origin',(-82.,38.3,29.1)) ;
#14070 = CARTESIAN_POINT('',(-81.25,38.3,29.1)) ;
#14071 = CARTESIAN_POINT('',(-81.25,38.3,29.1)) ;
#14072 = CARTESIAN_POINT('',(6.,38.3,29.1)) ;
#14073 = CARTESIAN_POINT('',(-82.,38.3,29.1)) ;
#14074 = CARTESIAN_POINT('',(6.,38.3,29.1)) ;
#14075 = CARTESIAN_POINT('Origin',(6.,38.3,29.1)) ;
#14076 = CARTESIAN_POINT('',(6.,49.3,29.1)) ;
#14077 = CARTESIAN_POINT('',(6.,38.3,29.1)) ;
#14078 = CARTESIAN_POINT('',(6.,49.3,29.1)) ;
#14079 = CARTESIAN_POINT('Origin',(-78.25,-52.3,29.1)) ;
#14080 = CARTESIAN_POINT('',(-87.25,-59.3,29.1)) ;
#14081 = CARTESIAN_POINT('',(-87.25,-45.3,29.1)) ;
#14082 = CARTESIAN_POINT('',(-69.25,-59.3,29.1)) ;
#14083 = CARTESIAN_POINT('',(-87.25,-59.3,29.1)) ;
#14084 = CARTESIAN_POINT('',(-69.25,-59.3,29.1)) ;
#14085 = CARTESIAN_POINT('Origin',(-69.25,-45.3,27.6)) ;
#14086 = CARTESIAN_POINT('',(-87.25,-45.3,29.1)) ;
#14087 = CARTESIAN_POINT('',(-87.25,-45.3,27.6)) ;
#14088 = CARTESIAN_POINT('',(-69.25,-45.3,29.1)) ;
#14089 = CARTESIAN_POINT('',(-34.625,-45.3,29.1)) ;
#14090 = CARTESIAN_POINT('',(-69.25,-45.3,27.6)) ;
#14091 = CARTESIAN_POINT('Origin',(-69.25,-59.3,27.6)) ;
#14092 = CARTESIAN_POINT('',(-69.25,-59.3,29.1)) ;
#14093 = CARTESIAN_POINT('',(-69.25,-59.3,27.6)) ;
#14094 = CARTESIAN_POINT('Origin',(-87.25,-59.3,27.6)) ;
#14095 = CARTESIAN_POINT('',(-87.25,-59.3,27.6)) ;
#14096 = CARTESIAN_POINT('Origin',(-78.25,52.3,29.1)) ;
#14097 = CARTESIAN_POINT('',(-69.25,59.3,29.1)) ;
#14098 = CARTESIAN_POINT('',(-69.25,45.3,29.1)) ;
#14099 = CARTESIAN_POINT('',(-87.25,59.3,29.1)) ;
#14100 = CARTESIAN_POINT('',(-69.25,59.3,29.1)) ;
#14101 = CARTESIAN_POINT('',(-87.25,59.3,29.1)) ;
#14102 = CARTESIAN_POINT('Origin',(-69.25,59.3,27.6)) ;
#14103 = CARTESIAN_POINT('',(-87.25,59.3,27.6)) ;
#14104 = CARTESIAN_POINT('',(-69.25,59.3,27.6)) ;
#14105 = CARTESIAN_POINT('Origin',(-69.25,45.3,27.6)) ;
#14106 = CARTESIAN_POINT('',(-69.25,45.3,29.1)) ;
#14107 = CARTESIAN_POINT('',(-69.25,48.8,29.1)) ;
#14108 = CARTESIAN_POINT('',(-69.25,45.3,27.6)) ;
#14109 = CARTESIAN_POINT('Origin',(-87.25,45.3,27.6)) ;
#14110 = CARTESIAN_POINT('',(-87.25,45.3,29.1)) ;
#14111 = CARTESIAN_POINT('',(-87.25,45.3,29.1)) ;
#14112 = CARTESIAN_POINT('',(-87.25,45.3,27.6)) ;
#14113 = CARTESIAN_POINT('Origin',(0.,52.3,29.1)) ;
#14114 = CARTESIAN_POINT('',(-87.25,55.3,29.1)) ;
#14115 = CARTESIAN_POINT('',(69.25,49.3,29.1)) ;
#14116 = CARTESIAN_POINT('',(69.25,55.8,29.1)) ;
#14117 = CARTESIAN_POINT('',(-87.25,49.3,29.1)) ;
#14118 = CARTESIAN_POINT('',(-81.25,-49.3,29.1)) ;
#14119 = CARTESIAN_POINT('',(69.25,-49.3,29.1)) ;
#14120 = CARTESIAN_POINT('',(87.25,-49.3,29.1)) ;
#14121 = CARTESIAN_POINT('',(69.25,3.5,29.1)) ;
#14122 = CARTESIAN_POINT('Origin',(-81.25,-49.3,29.1)) ;
#14123 = CARTESIAN_POINT('',(-81.25,49.3,39.1)) ;
#14124 = CARTESIAN_POINT('',(-81.25,49.3,29.1)) ;
#14125 = CARTESIAN_POINT('',(-81.25,-49.3,39.1)) ;
#14126 = CARTESIAN_POINT('',(-81.25,-49.3,39.1)) ;
#14127 = CARTESIAN_POINT('',(-81.25,-49.3,29.1)) ;
#14128 = CARTESIAN_POINT('Origin',(-87.25,49.3,29.1)) ;
#14129 = CARTESIAN_POINT('',(-87.25,49.3,29.1)) ;
#14130 = CARTESIAN_POINT('',(-87.25,49.3,39.1)) ;
#14131 = CARTESIAN_POINT('Origin',(78.25,-52.3,29.1)) ;
#14132 = CARTESIAN_POINT('',(69.25,-59.3,29.1)) ;
#14133 = CARTESIAN_POINT('',(69.25,-45.3,29.1)) ;
#14134 = CARTESIAN_POINT('',(69.25,-59.3,29.1)) ;
#14135 = CARTESIAN_POINT('Origin',(87.25,-45.3,27.6)) ;
#14136 = CARTESIAN_POINT('',(69.25,-45.3,29.1)) ;
#14137 = CARTESIAN_POINT('',(69.25,-45.3,27.6)) ;
#14138 = CARTESIAN_POINT('',(87.25,-45.3,29.1)) ;
#14139 = CARTESIAN_POINT('',(43.625,-45.3,29.1)) ;
#14140 = CARTESIAN_POINT('Origin',(69.25,-59.3,27.6)) ;
#14141 = CARTESIAN_POINT('',(69.25,-59.3,27.6)) ;
#14142 = CARTESIAN_POINT('Origin',(69.25,-45.3,27.6)) ;
#14143 = CARTESIAN_POINT('',(69.25,-45.3,29.1)) ;
#14144 = CARTESIAN_POINT('Origin',(78.25,-52.3,29.1)) ;
#14145 = CARTESIAN_POINT('',(87.25,-49.3,29.1)) ;
#14146 = CARTESIAN_POINT('Origin',(0.,52.3,29.1)) ;
#14147 = CARTESIAN_POINT('',(34.625,45.3,29.1)) ;
#14148 = CARTESIAN_POINT('Origin',(78.25,52.3,29.1)) ;
#14149 = CARTESIAN_POINT('',(69.25,59.3,29.1)) ;
#14150 = CARTESIAN_POINT('',(87.25,59.3,29.1)) ;
#14151 = CARTESIAN_POINT('',(69.25,59.3,29.1)) ;
#14152 = CARTESIAN_POINT('Origin',(78.25,52.3,29.1)) ;
#14153 = CARTESIAN_POINT('',(69.25,45.3,29.1)) ;
#14154 = CARTESIAN_POINT('',(69.25,59.3,29.1)) ;
#14155 = CARTESIAN_POINT('',(69.25,45.3,29.1)) ;
#14156 = CARTESIAN_POINT('Origin',(87.25,59.3,27.6)) ;
#14157 = CARTESIAN_POINT('',(69.25,59.3,27.6)) ;
#14158 = CARTESIAN_POINT('Origin',(69.25,45.3,27.6)) ;
#14159 = CARTESIAN_POINT('',(69.25,45.3,27.6)) ;
#14160 = CARTESIAN_POINT('Origin',(69.25,59.3,27.6)) ;
#14161 = CARTESIAN_POINT('Origin',(87.25,-49.3,29.1)) ;
#14162 = CARTESIAN_POINT('',(87.25,-49.3,39.1)) ;
#14163 = CARTESIAN_POINT('Origin',(-87.25,55.3,29.1)) ;
#14164 = CARTESIAN_POINT('',(-87.25,55.3,39.1)) ;
#14165 = CARTESIAN_POINT('Origin',(0.,52.3,39.1)) ;
#14166 = CARTESIAN_POINT('',(0.,0.,0.)) ;
#14167 = CARTESIAN_POINT('Origin',(72.,-50.7,44.4)) ;
#14168 = CARTESIAN_POINT('',(69.95,48.2,44.4)) ;
#14169 = CARTESIAN_POINT('Origin',(72.,48.2,44.4)) ;
#14170 = CARTESIAN_POINT('',(69.95,50.2,44.4)) ;
#14171 = CARTESIAN_POINT('',(69.95,-50.7,44.4)) ;
#14172 = CARTESIAN_POINT('Origin',(72.,50.2,44.4)) ;
#14173 = CARTESIAN_POINT('Origin',(72.,-50.7,44.4)) ;
#14174 = CARTESIAN_POINT('',(69.95,-50.2,44.4)) ;
#14175 = CARTESIAN_POINT('Origin',(72.,-50.2,44.4)) ;
#14176 = CARTESIAN_POINT('',(69.95,-48.2,44.4)) ;
#14177 = CARTESIAN_POINT('',(69.95,-50.7,44.4)) ;
#14178 = CARTESIAN_POINT('Origin',(72.,-48.2,44.4)) ;
#14179 = CARTESIAN_POINT('Origin',(72.,-48.2,44.15)) ;
#14180 = CARTESIAN_POINT('',(78.,-48.2,48.4)) ;
#14181 = CARTESIAN_POINT('',(66.,-48.2,48.4)) ;
#14182 = CARTESIAN_POINT('',(36.,-48.2,48.4)) ;
#14183 = CARTESIAN_POINT('',(78.,-48.2,39.4)) ;
#14184 = CARTESIAN_POINT('',(78.,-48.2,39.4)) ;
#14185 = CARTESIAN_POINT('',(66.,-48.2,39.4)) ;
#14186 = CARTESIAN_POINT('',(66.,-48.2,39.4)) ;
#14187 = CARTESIAN_POINT('',(66.,-48.2,48.9)) ;
#14188 = CARTESIAN_POINT('Origin',(78.,-50.2,48.9)) ;
#14189 = CARTESIAN_POINT('',(78.,-49.35,48.4)) ;
#14190 = CARTESIAN_POINT('',(78.,-25.1,48.4)) ;
#14191 = CARTESIAN_POINT('',(78.,-49.35,43.4)) ;
#14192 = CARTESIAN_POINT('',(78.,-49.35,43.4)) ;
#14193 = CARTESIAN_POINT('',(78.,-50.2,43.4)) ;
#14194 = CARTESIAN_POINT('',(78.,-25.1,43.4)) ;
#14195 = CARTESIAN_POINT('',(78.,-50.2,39.4)) ;
#14196 = CARTESIAN_POINT('',(78.,-50.2,39.4)) ;
#14197 = CARTESIAN_POINT('',(78.,-50.2,39.4)) ;
#14198 = CARTESIAN_POINT('Origin',(66.,-50.2,39.4)) ;
#14199 = CARTESIAN_POINT('',(66.,-50.2,48.4)) ;
#14200 = CARTESIAN_POINT('',(66.,-25.1,48.4)) ;
#14201 = CARTESIAN_POINT('',(66.,-50.2,39.4)) ;
#14202 = CARTESIAN_POINT('',(66.,-50.2,39.4)) ;
#14203 = CARTESIAN_POINT('',(66.,-50.2,48.9)) ;
#14204 = CARTESIAN_POINT('Origin',(78.,-50.2,39.4)) ;
#14205 = CARTESIAN_POINT('',(66.,-50.2,39.4)) ;
#14206 = CARTESIAN_POINT('Origin',(72.,-50.2,44.15)) ;
#14207 = CARTESIAN_POINT('',(77.1902194281898,-50.2,48.4)) ;
#14208 = CARTESIAN_POINT('',(36.,-50.2,48.4)) ;
#14209 = CARTESIAN_POINT('',(77.1902194281898,-50.2,43.4)) ;
#14210 = CARTESIAN_POINT('',(36.,-50.2,43.4)) ;
#14211 = CARTESIAN_POINT('',(77.1902194281898,-50.2,43.4)) ;
#14212 = CARTESIAN_POINT('Origin',(74.,-46.35,43.4)) ;
#14213 = CARTESIAN_POINT('',(79.,-46.35,48.4)) ;
#14214 = CARTESIAN_POINT('Origin',(74.,-46.35,48.4)) ;
#14215 = CARTESIAN_POINT('',(79.,-46.35,43.4)) ;
#14216 = CARTESIAN_POINT('',(79.,-46.35,43.4)) ;
#14217 = CARTESIAN_POINT('Origin',(74.,-46.35,43.4)) ;
#14218 = CARTESIAN_POINT('Origin',(74.,-46.35,43.4)) ;
#14219 = CARTESIAN_POINT('',(74.,-51.35,43.4)) ;
#14220 = CARTESIAN_POINT('Origin',(74.,-46.35,43.4)) ;
#14221 = CARTESIAN_POINT('',(74.,-51.35,48.4)) ;
#14222 = CARTESIAN_POINT('',(74.,-51.35,43.4)) ;
#14223 = CARTESIAN_POINT('Origin',(74.,-46.35,48.4)) ;
#14224 = CARTESIAN_POINT('Origin',(0.,0.,43.4)) ;
#14225 = CARTESIAN_POINT('',(-80.,-46.35,43.4)) ;
#14226 = CARTESIAN_POINT('',(-74.,-52.35,43.4)) ;
#14227 = CARTESIAN_POINT('Origin',(-74.,-46.35,43.4)) ;
#14228 = CARTESIAN_POINT('',(-80.,46.35,43.4)) ;
#14229 = CARTESIAN_POINT('',(-80.,46.35,43.4)) ;
#14230 = CARTESIAN_POINT('',(-74.,52.35,43.4)) ;
#14231 = CARTESIAN_POINT('Origin',(-74.,46.35,43.4)) ;
#14232 = CARTESIAN_POINT('',(74.,52.35,43.4)) ;
#14233 = CARTESIAN_POINT('',(74.,52.35,43.4)) ;
#14234 = CARTESIAN_POINT('',(80.,46.35,43.4)) ;
#14235 = CARTESIAN_POINT('Origin',(74.,46.35,43.4)) ;
#14236 = CARTESIAN_POINT('',(80.,-46.35,43.4)) ;
#14237 = CARTESIAN_POINT('',(80.,-46.35,43.4)) ;
#14238 = CARTESIAN_POINT('',(74.,-52.35,43.4)) ;
#14239 = CARTESIAN_POINT('Origin',(74.,-46.35,43.4)) ;
#14240 = CARTESIAN_POINT('',(-74.,-52.35,43.4)) ;
#14241 = CARTESIAN_POINT('',(79.,46.35,43.4)) ;
#14242 = CARTESIAN_POINT('',(79.,-23.175,43.4)) ;
#14243 = CARTESIAN_POINT('',(78.,49.35,43.4)) ;
#14244 = CARTESIAN_POINT('Origin',(74.,46.35,43.4)) ;
#14245 = CARTESIAN_POINT('',(78.,50.2,43.4)) ;
#14246 = CARTESIAN_POINT('',(78.,24.1,43.4)) ;
#14247 = CARTESIAN_POINT('',(77.1902194281898,50.2,43.4)) ;
#14248 = CARTESIAN_POINT('',(36.,50.2,43.4)) ;
#14249 = CARTESIAN_POINT('',(74.,51.35,43.4)) ;
#14250 = CARTESIAN_POINT('Origin',(74.,46.35,43.4)) ;
#14251 = CARTESIAN_POINT('',(-74.,51.35,43.4)) ;
#14252 = CARTESIAN_POINT('',(37.,51.35,43.4)) ;
#14253 = CARTESIAN_POINT('',(-79.,46.35,43.4)) ;
#14254 = CARTESIAN_POINT('Origin',(-74.,46.35,43.4)) ;
#14255 = CARTESIAN_POINT('',(-79.,-46.35,43.4)) ;
#14256 = CARTESIAN_POINT('',(-79.,23.175,43.4)) ;
#14257 = CARTESIAN_POINT('',(-74.,-51.35,43.4)) ;
#14258 = CARTESIAN_POINT('Origin',(-74.,-46.35,43.4)) ;
#14259 = CARTESIAN_POINT('',(-37.,-51.35,43.4)) ;
#14260 = CARTESIAN_POINT('Origin',(72.,48.2,44.15)) ;
#14261 = CARTESIAN_POINT('',(66.,48.2,48.4)) ;
#14262 = CARTESIAN_POINT('',(78.,48.2,48.4)) ;
#14263 = CARTESIAN_POINT('',(36.,48.2,48.4)) ;
#14264 = CARTESIAN_POINT('',(66.,48.2,39.4)) ;
#14265 = CARTESIAN_POINT('',(66.,48.2,48.9)) ;
#14266 = CARTESIAN_POINT('',(78.,48.2,39.4)) ;
#14267 = CARTESIAN_POINT('',(66.,48.2,39.4)) ;
#14268 = CARTESIAN_POINT('',(78.,48.2,39.4)) ;
#14269 = CARTESIAN_POINT('Origin',(66.,48.2,39.4)) ;
#14270 = CARTESIAN_POINT('',(66.,50.2,48.4)) ;
#14271 = CARTESIAN_POINT('',(66.,24.1,48.4)) ;
#14272 = CARTESIAN_POINT('',(66.,50.2,39.4)) ;
#14273 = CARTESIAN_POINT('',(66.,50.2,48.9)) ;
#14274 = CARTESIAN_POINT('',(66.,48.2,39.4)) ;
#14275 = CARTESIAN_POINT('Origin',(72.,50.2,44.15)) ;
#14276 = CARTESIAN_POINT('',(77.1902194281898,50.2,48.4)) ;
#14277 = CARTESIAN_POINT('',(36.,50.2,48.4)) ;
#14278 = CARTESIAN_POINT('',(77.1902194281898,50.2,43.4)) ;
#14279 = CARTESIAN_POINT('',(78.,50.2,39.4)) ;
#14280 = CARTESIAN_POINT('',(78.,50.2,39.4)) ;
#14281 = CARTESIAN_POINT('',(66.,50.2,39.4)) ;
#14282 = CARTESIAN_POINT('Origin',(78.,48.2,39.4)) ;
#14283 = CARTESIAN_POINT('',(78.,48.2,39.4)) ;
#14284 = CARTESIAN_POINT('Origin',(78.,48.2,48.9)) ;
#14285 = CARTESIAN_POINT('',(78.,49.35,48.4)) ;
#14286 = CARTESIAN_POINT('',(78.,24.1,48.4)) ;
#14287 = CARTESIAN_POINT('',(78.,49.35,43.4)) ;
#14288 = CARTESIAN_POINT('Origin',(74.,46.35,43.4)) ;
#14289 = CARTESIAN_POINT('',(74.,51.35,48.4)) ;
#14290 = CARTESIAN_POINT('Origin',(74.,46.35,48.4)) ;
#14291 = CARTESIAN_POINT('',(74.,51.35,43.4)) ;
#14292 = CARTESIAN_POINT('Origin',(74.,46.35,43.4)) ;
#14293 = CARTESIAN_POINT('',(79.,46.35,48.4)) ;
#14294 = CARTESIAN_POINT('',(79.,46.35,43.4)) ;
#14295 = CARTESIAN_POINT('Origin',(74.,46.35,48.4)) ;
#14296 = CARTESIAN_POINT('Origin',(-79.5,23.175,48.9)) ;
#14297 = CARTESIAN_POINT('',(-79.5,46.35,49.4)) ;
#14298 = CARTESIAN_POINT('',(-80.,46.35,48.9)) ;
#14299 = CARTESIAN_POINT('Origin',(-79.5,46.35,48.9)) ;
#14300 = CARTESIAN_POINT('',(-80.,-46.35,48.9)) ;
#14301 = CARTESIAN_POINT('',(-80.,23.175,48.9)) ;
#14302 = CARTESIAN_POINT('',(-79.5,-46.35,49.4)) ;
#14303 = CARTESIAN_POINT('Origin',(-79.5,-46.35,48.9)) ;
#14304 = CARTESIAN_POINT('',(-79.5,23.175,49.4)) ;
#14305 = CARTESIAN_POINT('Origin',(-74.,-46.35,48.9)) ;
#14306 = CARTESIAN_POINT('',(-74.,-52.35,48.9)) ;
#14307 = CARTESIAN_POINT('',(-74.,-51.85,49.4)) ;
#14308 = CARTESIAN_POINT('Origin',(-74.,-51.85,48.9)) ;
#14309 = CARTESIAN_POINT('Origin',(-74.,-46.35,49.4)) ;
#14310 = CARTESIAN_POINT('Origin',(-74.,-46.35,48.9)) ;
#14311 = CARTESIAN_POINT('Origin',(-37.,-51.85,48.9)) ;
#14312 = CARTESIAN_POINT('',(74.,-52.35,48.9)) ;
#14313 = CARTESIAN_POINT('',(74.,-51.85,49.4)) ;
#14314 = CARTESIAN_POINT('Origin',(74.,-51.85,48.9)) ;
#14315 = CARTESIAN_POINT('',(-37.,-51.85,49.4)) ;
#14316 = CARTESIAN_POINT('',(-37.,-52.35,48.9)) ;
#14317 = CARTESIAN_POINT('Origin',(74.,-46.35,48.9)) ;
#14318 = CARTESIAN_POINT('',(80.,-46.35,48.9)) ;
#14319 = CARTESIAN_POINT('',(79.5,-46.35,49.4)) ;
#14320 = CARTESIAN_POINT('Origin',(79.5,-46.35,48.9)) ;
#14321 = CARTESIAN_POINT('Origin',(74.,-46.35,49.4)) ;
#14322 = CARTESIAN_POINT('Origin',(74.,-46.35,48.9)) ;
#14323 = CARTESIAN_POINT('Origin',(79.5,-23.175,48.9)) ;
#14324 = CARTESIAN_POINT('',(80.,46.35,48.9)) ;
#14325 = CARTESIAN_POINT('',(79.5,46.35,49.4)) ;
#14326 = CARTESIAN_POINT('Origin',(79.5,46.35,48.9)) ;
#14327 = CARTESIAN_POINT('',(79.5,-23.175,49.4)) ;
#14328 = CARTESIAN_POINT('',(80.,-23.175,48.9)) ;
#14329 = CARTESIAN_POINT('Origin',(74.,46.35,48.9)) ;
#14330 = CARTESIAN_POINT('',(74.,52.35,48.9)) ;
#14331 = CARTESIAN_POINT('',(74.,51.85,49.4)) ;
#14332 = CARTESIAN_POINT('Origin',(74.,51.85,48.9)) ;
#14333 = CARTESIAN_POINT('Origin',(74.,46.35,49.4)) ;
#14334 = CARTESIAN_POINT('Origin',(74.,46.35,48.9)) ;
#14335 = CARTESIAN_POINT('Origin',(37.,51.85,48.9)) ;
#14336 = CARTESIAN_POINT('',(-74.,52.35,48.9)) ;
#14337 = CARTESIAN_POINT('',(-74.,51.85,49.4)) ;
#14338 = CARTESIAN_POINT('Origin',(-74.,51.85,48.9)) ;
#14339 = CARTESIAN_POINT('',(37.,51.85,49.4)) ;
#14340 = CARTESIAN_POINT('',(37.,52.35,48.9)) ;
#14341 = CARTESIAN_POINT('Origin',(-74.,46.35,48.9)) ;
#14342 = CARTESIAN_POINT('Origin',(-74.,46.35,49.4)) ;
#14343 = CARTESIAN_POINT('Origin',(-74.,46.35,48.9)) ;
#14344 = CARTESIAN_POINT('Origin',(74.,-46.35,43.4)) ;
#14345 = CARTESIAN_POINT('',(74.,-52.35,43.4)) ;
#14346 = CARTESIAN_POINT('',(80.,-46.35,43.4)) ;
#14347 = CARTESIAN_POINT('Origin',(-74.,-52.35,43.4)) ;
#14348 = CARTESIAN_POINT('',(-74.,-52.35,43.4)) ;
#14349 = CARTESIAN_POINT('Origin',(-74.,-46.35,43.4)) ;
#14350 = CARTESIAN_POINT('',(-80.,-46.35,43.4)) ;
#14351 = CARTESIAN_POINT('Origin',(-80.,46.35,43.4)) ;
#14352 = CARTESIAN_POINT('',(-80.,46.35,43.4)) ;
#14353 = CARTESIAN_POINT('Origin',(0.,0.,49.4)) ;
#14354 = CARTESIAN_POINT('Origin',(-79.,46.35,43.4)) ;
#14355 = CARTESIAN_POINT('',(-79.,46.35,48.4)) ;
#14356 = CARTESIAN_POINT('',(-79.,46.35,43.4)) ;
#14357 = CARTESIAN_POINT('',(-79.,-46.35,48.4)) ;
#14358 = CARTESIAN_POINT('',(-79.,46.35,48.4)) ;
#14359 = CARTESIAN_POINT('',(-79.,-46.35,43.4)) ;
#14360 = CARTESIAN_POINT('Origin',(-74.,46.35,43.4)) ;
#14361 = CARTESIAN_POINT('',(-74.,51.35,48.4)) ;
#14362 = CARTESIAN_POINT('',(-74.,51.35,43.4)) ;
#14363 = CARTESIAN_POINT('Origin',(-74.,46.35,48.4)) ;
#14364 = CARTESIAN_POINT('Origin',(74.,51.35,43.4)) ;
#14365 = CARTESIAN_POINT('',(74.,51.35,48.4)) ;
#14366 = CARTESIAN_POINT('Origin',(79.,-46.35,43.4)) ;
#14367 = CARTESIAN_POINT('',(79.,-46.35,48.4)) ;
#14368 = CARTESIAN_POINT('Origin',(-74.,-51.35,43.4)) ;
#14369 = CARTESIAN_POINT('',(-74.,-51.35,48.4)) ;
#14370 = CARTESIAN_POINT('',(-74.,-51.35,43.4)) ;
#14371 = CARTESIAN_POINT('',(-74.,-51.35,48.4)) ;
#14372 = CARTESIAN_POINT('Origin',(-74.,-46.35,43.4)) ;
#14373 = CARTESIAN_POINT('Origin',(-74.,-46.35,48.4)) ;
#14374 = CARTESIAN_POINT('Origin',(0.,0.,48.4)) ;
#14375 = CARTESIAN_POINT('Origin',(-74.,46.35,43.4)) ;
#14376 = CARTESIAN_POINT('',(-74.,52.35,43.4)) ;
#14377 = CARTESIAN_POINT('Origin',(74.,52.35,43.4)) ;
#14378 = CARTESIAN_POINT('',(74.,52.35,43.4)) ;
#14379 = CARTESIAN_POINT('Origin',(74.,46.35,43.4)) ;
#14380 = CARTESIAN_POINT('',(80.,46.35,43.4)) ;
#14381 = CARTESIAN_POINT('Origin',(80.,-46.35,43.4)) ;
#14382 = CARTESIAN_POINT('',(0.,0.,0.)) ;
#14383 = CARTESIAN_POINT('Origin',(-64.7118177099031,-45.3,43.8813793103448)) ;
#14384 = CARTESIAN_POINT('',(-67.2118177099031,44.8,43.8813793103448)) ;
#14385 = CARTESIAN_POINT('Origin',(-64.7118177099031,44.8,43.8813793103448)) ;
#14386 = CARTESIAN_POINT('',(-67.2118177099031,-44.8,43.8813793103448)) ;
#14387 = CARTESIAN_POINT('',(-67.2118177099031,-45.3,43.8813793103448)) ;
#14388 = CARTESIAN_POINT('Origin',(-64.7118177099031,-44.8,43.8813793103448)) ;
#14389 = CARTESIAN_POINT('Origin',(-72.6949895469778,-47.8,44.4)) ;
#14390 = CARTESIAN_POINT('',(-74.1949895469778,-44.8,44.4)) ;
#14391 = CARTESIAN_POINT('Origin',(-72.6949895469778,-44.8,44.4)) ;
#14392 = CARTESIAN_POINT('',(-74.1949895469778,-47.8,44.4)) ;
#14393 = CARTESIAN_POINT('',(-74.1949895469778,-47.8,44.4)) ;
#14394 = CARTESIAN_POINT('Origin',(-72.6949895469778,-47.8,44.4)) ;
#14395 = CARTESIAN_POINT('Origin',(-0.347494773488876,-47.8,39.7)) ;
#14396 = CARTESIAN_POINT('',(-2.39749477348887,-44.8,39.7)) ;
#14397 = CARTESIAN_POINT('Origin',(-0.347494773488876,-44.8,39.7)) ;
#14398 = CARTESIAN_POINT('',(-2.39749477348888,-47.8,39.7)) ;
#14399 = CARTESIAN_POINT('',(-2.39749477348888,-47.8,39.7)) ;
#14400 = CARTESIAN_POINT('Origin',(-0.347494773488876,-47.8,39.7)) ;
#14401 = CARTESIAN_POINT('Origin',(72.,-47.8,35.)) ;
#14402 = CARTESIAN_POINT('',(69.95,-44.8,35.)) ;
#14403 = CARTESIAN_POINT('Origin',(72.,-44.8,35.)) ;
#14404 = CARTESIAN_POINT('',(69.95,-47.8,35.)) ;
#14405 = CARTESIAN_POINT('',(69.95,-47.8,35.)) ;
#14406 = CARTESIAN_POINT('Origin',(72.,-47.8,35.)) ;
#14407 = CARTESIAN_POINT('Origin',(-72.4486447193915,-47.8,48.1920066226104)) ;
#14408 = CARTESIAN_POINT('',(-72.4486447193915,-47.8,48.1920066226104)) ;
#14409 = CARTESIAN_POINT('',(72.2463448275862,-47.8,38.7920066226105)) ;
#14410 = CARTESIAN_POINT('',(-72.4486447193915,-47.8,48.1920066226104)) ;
#14411 = CARTESIAN_POINT('',(72.2463448275862,-44.8,38.7920066226105)) ;
#14412 = CARTESIAN_POINT('',(72.2463448275862,-47.8,38.7920066226105)) ;
#14413 = CARTESIAN_POINT('',(-72.4486447193915,-44.8,48.1920066226104)) ;
#14414 = CARTESIAN_POINT('',(-72.4486447193915,-44.8,48.1920066226104)) ;
#14415 = CARTESIAN_POINT('',(-72.4486447193915,-47.8,48.1920066226104)) ;
#14416 = CARTESIAN_POINT('Origin',(-72.6949895469778,-47.8,44.4)) ;
#14417 = CARTESIAN_POINT('',(-72.941334374564,-47.8,40.6079933773895)) ;
#14418 = CARTESIAN_POINT('Origin',(-72.6949895469778,-47.8,44.4)) ;
#14419 = CARTESIAN_POINT('',(-72.941334374564,-44.8,40.6079933773895)) ;
#14420 = CARTESIAN_POINT('Origin',(-72.6949895469778,-44.8,44.4)) ;
#14421 = CARTESIAN_POINT('',(-72.941334374564,-47.8,40.6079933773895)) ;
#14422 = CARTESIAN_POINT('Origin',(71.7536551724138,-47.8,31.2079933773895)) ;
#14423 = CARTESIAN_POINT('',(71.7536551724138,-47.8,31.2079933773895)) ;
#14424 = CARTESIAN_POINT('',(71.7536551724138,-47.8,31.2079933773895)) ;
#14425 = CARTESIAN_POINT('',(71.7536551724138,-44.8,31.2079933773895)) ;
#14426 = CARTESIAN_POINT('',(71.7536551724138,-44.8,31.2079933773895)) ;
#14427 = CARTESIAN_POINT('',(71.7536551724138,-47.8,31.2079933773895)) ;
#14428 = CARTESIAN_POINT('Origin',(72.,-47.8,35.)) ;
#14429 = CARTESIAN_POINT('Origin',(72.,-47.8,35.)) ;
#14430 = CARTESIAN_POINT('Origin',(72.,-44.8,35.)) ;
#14431 = CARTESIAN_POINT('Origin',(-0.347494773488872,-44.8,39.7)) ;
#14432 = CARTESIAN_POINT('Origin',(-0.347494773488872,-47.8,39.7)) ;
#14433 = CARTESIAN_POINT('Origin',(-72.6949895469778,44.8,44.4)) ;
#14434 = CARTESIAN_POINT('',(-74.1949895469778,47.8,44.4)) ;
#14435 = CARTESIAN_POINT('Origin',(-72.6949895469778,47.8,44.4)) ;
#14436 = CARTESIAN_POINT('',(-74.1949895469778,44.8,44.4)) ;
#14437 = CARTESIAN_POINT('',(-74.1949895469778,44.8,44.4)) ;
#14438 = CARTESIAN_POINT('Origin',(-72.6949895469778,44.8,44.4)) ;
#14439 = CARTESIAN_POINT('Origin',(-0.347494773488876,44.8,39.7)) ;
#14440 = CARTESIAN_POINT('',(-2.39749477348887,47.8,39.7)) ;
#14441 = CARTESIAN_POINT('Origin',(-0.347494773488876,47.8,39.7)) ;
#14442 = CARTESIAN_POINT('',(-2.39749477348888,44.8,39.7)) ;
#14443 = CARTESIAN_POINT('',(-2.39749477348888,44.8,39.7)) ;
#14444 = CARTESIAN_POINT('Origin',(-0.347494773488876,44.8,39.7)) ;
#14445 = CARTESIAN_POINT('Origin',(72.,44.8,35.)) ;
#14446 = CARTESIAN_POINT('',(69.95,47.8,35.)) ;
#14447 = CARTESIAN_POINT('Origin',(72.,47.8,35.)) ;
#14448 = CARTESIAN_POINT('',(69.95,44.8,35.)) ;
#14449 = CARTESIAN_POINT('',(69.95,44.8,35.)) ;
#14450 = CARTESIAN_POINT('Origin',(72.,44.8,35.)) ;
#14451 = CARTESIAN_POINT('Origin',(-72.4486447193915,44.8,48.1920066226104)) ;
#14452 = CARTESIAN_POINT('',(-72.4486447193915,44.8,48.1920066226104)) ;
#14453 = CARTESIAN_POINT('',(72.2463448275862,44.8,38.7920066226105)) ;
#14454 = CARTESIAN_POINT('',(-72.4486447193915,44.8,48.1920066226104)) ;
#14455 = CARTESIAN_POINT('',(72.2463448275862,47.8,38.7920066226105)) ;
#14456 = CARTESIAN_POINT('',(72.2463448275862,44.8,38.7920066226105)) ;
#14457 = CARTESIAN_POINT('',(-72.4486447193915,47.8,48.1920066226104)) ;
#14458 = CARTESIAN_POINT('',(-72.4486447193915,47.8,48.1920066226104)) ;
#14459 = CARTESIAN_POINT('',(-72.4486447193915,44.8,48.1920066226104)) ;
#14460 = CARTESIAN_POINT('Origin',(-72.6949895469778,44.8,44.4)) ;
#14461 = CARTESIAN_POINT('',(-72.941334374564,44.8,40.6079933773895)) ;
#14462 = CARTESIAN_POINT('Origin',(-72.6949895469778,44.8,44.4)) ;
#14463 = CARTESIAN_POINT('',(-72.941334374564,47.8,40.6079933773895)) ;
#14464 = CARTESIAN_POINT('Origin',(-72.6949895469778,47.8,44.4)) ;
#14465 = CARTESIAN_POINT('',(-72.941334374564,44.8,40.6079933773895)) ;
#14466 = CARTESIAN_POINT('Origin',(71.7536551724138,44.8,31.2079933773895)) ;
#14467 = CARTESIAN_POINT('',(71.7536551724138,44.8,31.2079933773895)) ;
#14468 = CARTESIAN_POINT('',(71.7536551724138,44.8,31.2079933773895)) ;
#14469 = CARTESIAN_POINT('',(71.7536551724138,47.8,31.2079933773895)) ;
#14470 = CARTESIAN_POINT('',(71.7536551724138,47.8,31.2079933773895)) ;
#14471 = CARTESIAN_POINT('',(71.7536551724138,44.8,31.2079933773895)) ;
#14472 = CARTESIAN_POINT('Origin',(72.,44.8,35.)) ;
#14473 = CARTESIAN_POINT('Origin',(72.,44.8,35.)) ;
#14474 = CARTESIAN_POINT('Origin',(72.,47.8,35.)) ;
#14475 = CARTESIAN_POINT('Origin',(-0.347494773488872,47.8,39.7)) ;
#14476 = CARTESIAN_POINT('Origin',(-0.347494773488872,44.8,39.7)) ;
#14477 = CARTESIAN_POINT('',(0.,0.,0.)) ;
#14478 = CARTESIAN_POINT('Origin',(22.1051760182835,-41.8,41.1586206896552)) ;
#14479 = CARTESIAN_POINT('',(19.6051760182835,41.3,41.1586206896552)) ;
#14480 = CARTESIAN_POINT('Origin',(22.1051760182835,41.3,41.1586206896552)) ;
#14481 = CARTESIAN_POINT('',(19.6051760182835,-41.3,41.1586206896552)) ;
#14482 = CARTESIAN_POINT('',(19.6051760182835,-41.8,41.1586206896552)) ;
#14483 = CARTESIAN_POINT('Origin',(22.1051760182835,-41.3,41.1586206896552)) ;
#14484 = CARTESIAN_POINT('Origin',(-64.7118177099031,-41.8,35.5186206896552)) ;
#14485 = CARTESIAN_POINT('',(-67.2118177099031,41.3,35.5186206896552)) ;
#14486 = CARTESIAN_POINT('Origin',(-64.7118177099031,41.3,35.5186206896552)) ;
#14487 = CARTESIAN_POINT('',(-67.2118177099031,-41.3,35.5186206896552)) ;
#14488 = CARTESIAN_POINT('',(-67.2118177099031,-41.8,35.5186206896552)) ;
#14489 = CARTESIAN_POINT('Origin',(-64.7118177099031,-41.3,35.5186206896552)) ;
#14490 = CARTESIAN_POINT('Origin',(72.,-44.3,44.4)) ;
#14491 = CARTESIAN_POINT('',(69.95,-41.3,44.4)) ;
#14492 = CARTESIAN_POINT('Origin',(72.,-41.3,44.4)) ;
#14493 = CARTESIAN_POINT('',(69.95,-44.3,44.4)) ;
#14494 = CARTESIAN_POINT('',(69.95,-44.3,44.4)) ;
#14495 = CARTESIAN_POINT('Origin',(72.,-44.3,44.4)) ;
#14496 = CARTESIAN_POINT('Origin',(-72.6949895469778,-44.3,35.)) ;
#14497 = CARTESIAN_POINT('',(-74.1949895469778,-41.3,35.)) ;
#14498 = CARTESIAN_POINT('Origin',(-72.6949895469778,-41.3,35.)) ;
#14499 = CARTESIAN_POINT('',(-74.1949895469778,-44.3,35.)) ;
#14500 = CARTESIAN_POINT('',(-74.1949895469778,-44.3,35.)) ;
#14501 = CARTESIAN_POINT('Origin',(-72.6949895469778,-44.3,35.)) ;
#14502 = CARTESIAN_POINT('Origin',(-0.347494773488876,-44.3,39.7)) ;
#14503 = CARTESIAN_POINT('',(-2.39749477348888,-41.3,39.7)) ;
#14504 = CARTESIAN_POINT('Origin',(-0.347494773488876,-41.3,39.7)) ;
#14505 = CARTESIAN_POINT('',(-2.39749477348888,-44.3,39.7)) ;
#14506 = CARTESIAN_POINT('',(-2.39749477348888,-44.3,39.7)) ;
#14507 = CARTESIAN_POINT('Origin',(-0.347494773488876,-44.3,39.7)) ;
#14508 = CARTESIAN_POINT('Origin',(-72.941334374564,-44.3,38.7920066226105)) ;
#14509 = CARTESIAN_POINT('',(-72.941334374564,-44.3,38.7920066226105)) ;
#14510 = CARTESIAN_POINT('',(71.7536551724138,-44.3,48.1920066226104)) ;
#14511 = CARTESIAN_POINT('',(-72.941334374564,-44.3,38.7920066226105)) ;
#14512 = CARTESIAN_POINT('',(71.7536551724138,-41.3,48.1920066226104)) ;
#14513 = CARTESIAN_POINT('',(71.7536551724138,-44.3,48.1920066226104)) ;
#14514 = CARTESIAN_POINT('',(-72.941334374564,-41.3,38.7920066226105)) ;
#14515 = CARTESIAN_POINT('',(-72.941334374564,-41.3,38.7920066226105)) ;
#14516 = CARTESIAN_POINT('',(-72.941334374564,-44.3,38.7920066226105)) ;
#14517 = CARTESIAN_POINT('Origin',(-72.6949895469778,-44.3,35.)) ;
#14518 = CARTESIAN_POINT('',(-72.4486447193915,-44.3,31.2079933773895)) ;
#14519 = CARTESIAN_POINT('Origin',(-72.6949895469778,-44.3,35.)) ;
#14520 = CARTESIAN_POINT('',(-72.4486447193915,-41.3,31.2079933773895)) ;
#14521 = CARTESIAN_POINT('Origin',(-72.6949895469778,-41.3,35.)) ;
#14522 = CARTESIAN_POINT('',(-72.4486447193915,-44.3,31.2079933773895)) ;
#14523 = CARTESIAN_POINT('Origin',(72.2463448275862,-44.3,40.6079933773895)) ;
#14524 = CARTESIAN_POINT('',(72.2463448275862,-44.3,40.6079933773895)) ;
#14525 = CARTESIAN_POINT('',(72.2463448275862,-44.3,40.6079933773895)) ;
#14526 = CARTESIAN_POINT('',(72.2463448275862,-41.3,40.6079933773895)) ;
#14527 = CARTESIAN_POINT('',(72.2463448275862,-41.3,40.6079933773895)) ;
#14528 = CARTESIAN_POINT('',(72.2463448275862,-44.3,40.6079933773895)) ;
#14529 = CARTESIAN_POINT('Origin',(72.,-44.3,44.4)) ;
#14530 = CARTESIAN_POINT('Origin',(72.,-44.3,44.4)) ;
#14531 = CARTESIAN_POINT('Origin',(72.,-41.3,44.4)) ;
#14532 = CARTESIAN_POINT('Origin',(-0.347494773488863,-41.3,39.7)) ;
#14533 = CARTESIAN_POINT('Origin',(-0.347494773488863,-44.3,39.7)) ;
#14534 = CARTESIAN_POINT('Origin',(-72.6949895469778,41.3,35.)) ;
#14535 = CARTESIAN_POINT('',(-74.1949895469778,44.3,35.)) ;
#14536 = CARTESIAN_POINT('Origin',(-72.6949895469778,44.3,35.)) ;
#14537 = CARTESIAN_POINT('',(-74.1949895469778,41.3,35.)) ;
#14538 = CARTESIAN_POINT('',(-74.1949895469778,41.3,35.)) ;
#14539 = CARTESIAN_POINT('Origin',(-72.6949895469778,41.3,35.)) ;
#14540 = CARTESIAN_POINT('Origin',(72.,41.3,44.4)) ;
#14541 = CARTESIAN_POINT('',(69.95,44.3,44.4)) ;
#14542 = CARTESIAN_POINT('Origin',(72.,44.3,44.4)) ;
#14543 = CARTESIAN_POINT('',(69.95,41.3,44.4)) ;
#14544 = CARTESIAN_POINT('',(69.95,41.3,44.4)) ;
#14545 = CARTESIAN_POINT('Origin',(72.,41.3,44.4)) ;
#14546 = CARTESIAN_POINT('Origin',(-0.347494773488876,41.3,39.7)) ;
#14547 = CARTESIAN_POINT('',(-2.39749477348888,44.3,39.7)) ;
#14548 = CARTESIAN_POINT('Origin',(-0.347494773488876,44.3,39.7)) ;
#14549 = CARTESIAN_POINT('',(-2.39749477348888,41.3,39.7)) ;
#14550 = CARTESIAN_POINT('',(-2.39749477348888,41.3,39.7)) ;
#14551 = CARTESIAN_POINT('Origin',(-0.347494773488876,41.3,39.7)) ;
#14552 = CARTESIAN_POINT('Origin',(-72.941334374564,41.3,38.7920066226105)) ;
#14553 = CARTESIAN_POINT('',(-72.941334374564,41.3,38.7920066226105)) ;
#14554 = CARTESIAN_POINT('',(71.7536551724138,41.3,48.1920066226104)) ;
#14555 = CARTESIAN_POINT('',(-72.941334374564,41.3,38.7920066226105)) ;
#14556 = CARTESIAN_POINT('',(71.7536551724138,44.3,48.1920066226104)) ;
#14557 = CARTESIAN_POINT('',(71.7536551724138,41.3,48.1920066226104)) ;
#14558 = CARTESIAN_POINT('',(-72.941334374564,44.3,38.7920066226105)) ;
#14559 = CARTESIAN_POINT('',(-72.941334374564,44.3,38.7920066226105)) ;
#14560 = CARTESIAN_POINT('',(-72.941334374564,41.3,38.7920066226105)) ;
#14561 = CARTESIAN_POINT('Origin',(-72.6949895469778,41.3,35.)) ;
#14562 = CARTESIAN_POINT('',(-72.4486447193915,41.3,31.2079933773895)) ;
#14563 = CARTESIAN_POINT('Origin',(-72.6949895469778,41.3,35.)) ;
#14564 = CARTESIAN_POINT('',(-72.4486447193915,44.3,31.2079933773895)) ;
#14565 = CARTESIAN_POINT('Origin',(-72.6949895469778,44.3,35.)) ;
#14566 = CARTESIAN_POINT('',(-72.4486447193915,41.3,31.2079933773895)) ;
#14567 = CARTESIAN_POINT('Origin',(72.2463448275862,41.3,40.6079933773895)) ;
#14568 = CARTESIAN_POINT('',(72.2463448275862,41.3,40.6079933773895)) ;
#14569 = CARTESIAN_POINT('',(72.2463448275862,41.3,40.6079933773895)) ;
#14570 = CARTESIAN_POINT('',(72.2463448275862,44.3,40.6079933773895)) ;
#14571 = CARTESIAN_POINT('',(72.2463448275862,44.3,40.6079933773895)) ;
#14572 = CARTESIAN_POINT('',(72.2463448275862,41.3,40.6079933773895)) ;
#14573 = CARTESIAN_POINT('Origin',(72.,41.3,44.4)) ;
#14574 = CARTESIAN_POINT('Origin',(72.,41.3,44.4)) ;
#14575 = CARTESIAN_POINT('Origin',(72.,44.3,44.4)) ;
#14576 = CARTESIAN_POINT('Origin',(-0.347494773488863,44.3,39.7)) ;
#14577 = CARTESIAN_POINT('Origin',(-0.347494773488863,41.3,39.7)) ;
#14578 = CARTESIAN_POINT('',(0.,0.,0.)) ;
#14579 = CARTESIAN_POINT('Origin',(77.,-2.,35.)) ;
#14580 = CARTESIAN_POINT('',(74.,-1.97183411479483,35.000000000015)) ;
#14581 = CARTESIAN_POINT('',(74.,-2.,35.)) ;
#14582 = CARTESIAN_POINT('',(74.,-2.,35.)) ;
#14583 = CARTESIAN_POINT('',(74.0187033397783,-2.,35.3344700640584)) ;
#14584 = CARTESIAN_POINT('Origin',(77.,-2.,35.)) ;
#14585 = CARTESIAN_POINT('Ctrl Pts',(74.0187033397784,-1.99999999999999,35.3344700640584)) ;
#14586 = CARTESIAN_POINT('Ctrl Pts',(74.0064065326714,-1.99999999999999,35.224862556844)) ;
#14587 = CARTESIAN_POINT('Ctrl Pts',(74.0000000000011,-1.99077077040239,35.1123394944064)) ;
#14588 = CARTESIAN_POINT('Ctrl Pts',(74.,-1.97183411479483,35.0000000000301)) ;
#14589 = CARTESIAN_POINT('Origin',(77.,-2.,35.)) ;
#14590 = CARTESIAN_POINT('',(74.,2.,35.)) ;
#14591 = CARTESIAN_POINT('',(74.,1.97183411479483,35.000000000015)) ;
#14592 = CARTESIAN_POINT('',(74.,-2.,35.)) ;
#14593 = CARTESIAN_POINT('',(74.0187033397783,2.,35.3344700640584)) ;
#14594 = CARTESIAN_POINT('Origin',(77.,2.,35.)) ;
#14595 = CARTESIAN_POINT('',(75.0008527115894,-2.4492935982947E-16,37.2368303733722)) ;
#14596 = CARTESIAN_POINT('Ctrl Pts',(74.0187033397784,1.99999999999999,35.3344700640584)) ;
#14597 = CARTESIAN_POINT('Ctrl Pts',(74.0477046447873,1.99999999999999,35.5929730006627)) ;
#14598 = CARTESIAN_POINT('Ctrl Pts',(74.1144354069026,1.94624453140306,35.8591102084627)) ;
#14599 = CARTESIAN_POINT('Ctrl Pts',(74.3000163132069,1.73918232877706,36.3321566427019)) ;
#14600 = CARTESIAN_POINT('Ctrl Pts',(74.4178370345461,1.58626985902425,36.5396414824713)) ;
#14601 = CARTESIAN_POINT('Ctrl Pts',(74.6402213681462,1.24024335258715,36.862889628107)) ;
#14602 = CARTESIAN_POINT('Ctrl Pts',(74.7617847795615,1.02133350899655,37.0018504709194)) ;
#14603 = CARTESIAN_POINT('Ctrl Pts',(74.943978655708,0.533317960206907,37.1885590945277)) ;
#14604 = CARTESIAN_POINT('Ctrl Pts',(75.0008527115894,0.263018234644198,37.2368303733722)) ;
#14605 = CARTESIAN_POINT('Ctrl Pts',(75.0008527115894,5.55111512312578E-16,
37.2368303733722)) ;
#14606 = CARTESIAN_POINT('Ctrl Pts',(75.0008527115894,-1.38777878078145E-16,
37.2368303733722)) ;
#14607 = CARTESIAN_POINT('Ctrl Pts',(75.0008527115894,-0.263018234644197,
37.2368303733722)) ;
#14608 = CARTESIAN_POINT('Ctrl Pts',(74.943978655708,-0.533317960206906,37.1885590945277)) ;
#14609 = CARTESIAN_POINT('Ctrl Pts',(74.7617847795615,-1.02133350899655,37.0018504709194)) ;
#14610 = CARTESIAN_POINT('Ctrl Pts',(74.6402213681462,-1.24024335258715,36.862889628107)) ;
#14611 = CARTESIAN_POINT('Ctrl Pts',(74.4178370345462,-1.58626985902425,36.5396414824713)) ;
#14612 = CARTESIAN_POINT('Ctrl Pts',(74.3000163132069,-1.73918232877706,36.3321566427019)) ;
#14613 = CARTESIAN_POINT('Ctrl Pts',(74.1144354069026,-1.94624453140306,35.8591102084627)) ;
#14614 = CARTESIAN_POINT('Ctrl Pts',(74.0477046447873,-1.99999999999999,35.5929730006628)) ;
#14615 = CARTESIAN_POINT('Ctrl Pts',(74.0187033397784,-1.99999999999999,35.3344700640584)) ;
#14616 = CARTESIAN_POINT('Origin',(77.,-2.,35.)) ;
#14617 = CARTESIAN_POINT('Ctrl Pts',(74.,-1.97183411479483,35.0000000000301)) ;
#14618 = CARTESIAN_POINT('Ctrl Pts',(73.9999999999985,-1.94610976853832,34.8473933248331)) ;
#14619 = CARTESIAN_POINT('Ctrl Pts',(74.0119436372818,-1.90234643847172,34.6951462661377)) ;
#14620 = CARTESIAN_POINT('Ctrl Pts',(74.0719456039354,-1.73918232877706,34.2992499137851)) ;
#14621 = CARTESIAN_POINT('Ctrl Pts',(74.1408607543884,-1.58626985902425,34.0708152772934)) ;
#14622 = CARTESIAN_POINT('Ctrl Pts',(74.2860880828058,-1.24024335258715,33.706324977603)) ;
#14623 = CARTESIAN_POINT('Ctrl Pts',(74.3738371045158,-1.02133350899655,33.5438814858313)) ;
#14624 = CARTESIAN_POINT('Ctrl Pts',(74.5101288893078,-0.533317960206906,
33.3214421277285)) ;
#14625 = CARTESIAN_POINT('Ctrl Pts',(74.5548926261781,-0.263018234644197,
33.2617681597434)) ;
#14626 = CARTESIAN_POINT('Ctrl Pts',(74.5548926261781,0.,33.2617681597434)) ;
#14627 = CARTESIAN_POINT('Ctrl Pts',(74.5548926261781,0.263018234644197,33.2617681597434)) ;
#14628 = CARTESIAN_POINT('Ctrl Pts',(74.5101288893078,0.533317960206908,33.3214421277285)) ;
#14629 = CARTESIAN_POINT('Ctrl Pts',(74.3738371045158,1.02133350899655,33.5438814858313)) ;
#14630 = CARTESIAN_POINT('Ctrl Pts',(74.2860880828058,1.24024335258715,33.706324977603)) ;
#14631 = CARTESIAN_POINT('Ctrl Pts',(74.1408607543884,1.58626985902425,34.0708152772934)) ;
#14632 = CARTESIAN_POINT('Ctrl Pts',(74.0719456039354,1.73918232877707,34.2992499137851)) ;
#14633 = CARTESIAN_POINT('Ctrl Pts',(74.0119436372818,1.90234643847172,34.6951462661377)) ;
#14634 = CARTESIAN_POINT('Ctrl Pts',(73.9999999999985,1.94610976853832,34.8473933248331)) ;
#14635 = CARTESIAN_POINT('Ctrl Pts',(74.,1.97183411479483,35.0000000000301)) ;
#14636 = CARTESIAN_POINT('Origin',(77.,-2.5,35.)) ;
#14637 = CARTESIAN_POINT('',(74.95,-2.,35.)) ;
#14638 = CARTESIAN_POINT('Origin',(77.,-2.,35.)) ;
#14639 = CARTESIAN_POINT('',(74.95,2.,35.)) ;
#14640 = CARTESIAN_POINT('',(74.95,-2.5,35.)) ;
#14641 = CARTESIAN_POINT('Origin',(77.,2.,35.)) ;
#14642 = CARTESIAN_POINT('Origin',(67.5432559211121,0.,31.4320886465021)) ;
#14643 = CARTESIAN_POINT('',(68.568964117558,-5.63337527607782E-16,40.5747317378485)) ;
#14644 = CARTESIAN_POINT('Origin',(68.0561100193351,0.,36.0034101921753)) ;
#14645 = CARTESIAN_POINT('Origin',(48.1807989511907,0.,38.2332106192315)) ;
#14646 = CARTESIAN_POINT('',(28.8183419812693,-5.63337527607782E-16,45.0343325919609)) ;
#14647 = CARTESIAN_POINT('',(48.6936530494136,-5.63337527607782E-16,42.8045321649047)) ;
#14648 = CARTESIAN_POINT('Origin',(28.3054878830464,0.,40.4630110462877)) ;
#14649 = CARTESIAN_POINT('Origin',(28.0713588382055,0.,38.3761033841325)) ;
#14650 = CARTESIAN_POINT('',(28.5396169278873,-2.57175827820943E-16,42.5499187084428)) ;
#14651 = CARTESIAN_POINT('Origin',(28.3054878830464,0.,40.4630110462877)) ;
#14652 = CARTESIAN_POINT('Origin',(27.8086051063428,0.,40.5187560569641)) ;
#14653 = CARTESIAN_POINT('',(27.5458513744801,-2.57175827820943E-16,42.6614087297956)) ;
#14654 = CARTESIAN_POINT('',(28.0427341511837,-2.57175827820943E-16,42.6056637191192)) ;
#14655 = CARTESIAN_POINT('Origin',(27.3117223296392,0.,40.5745010676405)) ;
#14656 = CARTESIAN_POINT('Origin',(26.7542722228752,0.,35.6056733006044)) ;
#14657 = CARTESIAN_POINT('',(27.8691724364032,-6.12323399573676E-16,45.5433288346766)) ;
#14658 = CARTESIAN_POINT('Origin',(27.3117223296392,0.,40.5745010676405)) ;
#14659 = CARTESIAN_POINT('Origin',(48.1807989511907,0.,38.2332106192315)) ;
#14660 = CARTESIAN_POINT('',(69.6073256795063,-6.12323399573676E-16,40.8607479378586)) ;
#14661 = CARTESIAN_POINT('Origin',(69.0498755727423,0.,35.8919201708225)) ;
#14662 = CARTESIAN_POINT('',(48.7382490579548,-6.12323399573676E-16,43.2020383862676)) ;
#14663 = CARTESIAN_POINT('Origin',(68.8268955300367,0.,33.9043890640081)) ;
#14664 = CARTESIAN_POINT('',(69.2728556154479,-2.4492935982947E-16,37.8794512776369)) ;
#14665 = CARTESIAN_POINT('Origin',(69.0498755727423,0.,35.8919201708225)) ;
#14666 = CARTESIAN_POINT('Origin',(72.0311722329639,0.,35.557450106764)) ;
#14667 = CARTESIAN_POINT('Ctrl Pts',(74.,1.97183411479483,35.0000000000301)) ;
#14668 = CARTESIAN_POINT('Ctrl Pts',(74.0000000000011,1.99077077040239,35.1123394944064)) ;
#14669 = CARTESIAN_POINT('Ctrl Pts',(74.0064065326714,1.99999999999999,35.224862556844)) ;
#14670 = CARTESIAN_POINT('Ctrl Pts',(74.0187033397784,1.99999999999999,35.3344700640584)) ;
#14671 = CARTESIAN_POINT('',(72.2541522756695,-2.4492935982947E-16,37.5449812135785)) ;
#14672 = CARTESIAN_POINT('Origin',(77.,-2.,35.)) ;
#14673 = CARTESIAN_POINT('Origin',(77.,2.,35.)) ;
#14674 = CARTESIAN_POINT('Origin',(77.,2.,35.)) ;
#14675 = CARTESIAN_POINT('Origin',(77.,-2.,35.)) ;
#14676 = CARTESIAN_POINT('',(0.,0.,0.)) ;
#14677 = CARTESIAN_POINT('Origin',(22.1051760182835,-2.,41.1586206896552)) ;
#14678 = CARTESIAN_POINT('',(18.6051760182835,2.00000000000001,41.1586206896552)) ;
#14679 = CARTESIAN_POINT('',(18.6051760182835,-2.00000000000001,41.1586206896552)) ;
#14680 = CARTESIAN_POINT('',(18.6051760182835,-2.,41.1586206896552)) ;
#14681 = CARTESIAN_POINT('',(25.5833554552088,2.,40.7684056149203)) ;
#14682 = CARTESIAN_POINT('Origin',(22.1051760182835,2.,41.1586206896552)) ;
#14683 = CARTESIAN_POINT('',(24.8854811841601,0.866025403784449,39.032614296297)) ;
#14684 = CARTESIAN_POINT('Ctrl Pts',(24.8854811841601,0.866025403784446,39.032614296297)) ;
#14685 = CARTESIAN_POINT('Ctrl Pts',(24.9563991705139,1.07434212579119,39.1253579702713)) ;
#14686 = CARTESIAN_POINT('Ctrl Pts',(25.0451560272598,1.26170274467392,39.2522326008807)) ;
#14687 = CARTESIAN_POINT('Ctrl Pts',(25.2247815177785,1.58802031554125,39.5604452573204)) ;
#14688 = CARTESIAN_POINT('Ctrl Pts',(25.3282720606242,1.74115309287314,39.7711453733977)) ;
#14689 = CARTESIAN_POINT('Ctrl Pts',(25.4937233402356,1.94729108188327,40.2469283253369)) ;
#14690 = CARTESIAN_POINT('Ctrl Pts',(25.5546455359111,2.,40.5124999428882)) ;
#14691 = CARTESIAN_POINT('Ctrl Pts',(25.5833554552088,2.00000000000001,40.7684056149203)) ;
#14692 = CARTESIAN_POINT('',(24.8854811841601,-0.866025403784449,39.032614296297)) ;
#14693 = CARTESIAN_POINT('',(24.8854811841601,-2.,39.032614296297)) ;
#14694 = CARTESIAN_POINT('',(25.5833554552088,-2.,40.7684056149203)) ;
#14695 = CARTESIAN_POINT('Ctrl Pts',(25.5833554552088,-2.00000000000001,40.7684056149203)) ;
#14696 = CARTESIAN_POINT('Ctrl Pts',(25.5546455359111,-2.,40.5124999428882)) ;
#14697 = CARTESIAN_POINT('Ctrl Pts',(25.4937233402356,-1.94729108188327,40.2469283253369)) ;
#14698 = CARTESIAN_POINT('Ctrl Pts',(25.3282720606242,-1.74115309287314,39.7711453733977)) ;
#14699 = CARTESIAN_POINT('Ctrl Pts',(25.2247815177785,-1.58802031554125,39.5604452573204)) ;
#14700 = CARTESIAN_POINT('Ctrl Pts',(25.0451560272598,-1.26170274467392,39.2522326008807)) ;
#14701 = CARTESIAN_POINT('Ctrl Pts',(24.9563991705139,-1.07434212579119,39.1253579702713)) ;
#14702 = CARTESIAN_POINT('Ctrl Pts',(24.8854811841601,-0.866025403784446,
39.032614296297)) ;
#14703 = CARTESIAN_POINT('Origin',(22.1051760182835,-2.,41.1586206896552)) ;
#14704 = CARTESIAN_POINT('Origin',(22.1051760182835,-2.5,41.1586206896552)) ;
#14705 = CARTESIAN_POINT('',(19.5551760182835,-2.,41.1586206896552)) ;
#14706 = CARTESIAN_POINT('Origin',(22.1051760182835,-2.,41.1586206896552)) ;
#14707 = CARTESIAN_POINT('',(19.5551760182835,2.,41.1586206896552)) ;
#14708 = CARTESIAN_POINT('',(19.5551760182835,-2.5,41.1586206896552)) ;
#14709 = CARTESIAN_POINT('Origin',(22.1051760182835,2.,41.1586206896552)) ;
#14710 = CARTESIAN_POINT('Origin',(22.1051760182835,-2.,41.1586206896552)) ;
#14711 = CARTESIAN_POINT('Origin',(22.1051760182835,-2.,41.1586206896552)) ;
#14712 = CARTESIAN_POINT('',(25.2874641728502,-0.866025403784418,42.6156869548965)) ;
#14713 = CARTESIAN_POINT('Ctrl Pts',(25.2874641728502,-0.866025403784424,
42.6156869548965)) ;
#14714 = CARTESIAN_POINT('Ctrl Pts',(25.3360680744367,-1.07434212579117,42.5095341847899)) ;
#14715 = CARTESIAN_POINT('Ctrl Pts',(25.3945042964362,-1.26170274467391,42.3661460420789)) ;
#14716 = CARTESIAN_POINT('Ctrl Pts',(25.5013674810673,-1.58802031554125,42.0257923757197)) ;
#14717 = CARTESIAN_POINT('Ctrl Pts',(25.5555962292677,-1.74115309287314,41.7973978174612)) ;
#14718 = CARTESIAN_POINT('Ctrl Pts',(25.6115056919801,-1.94729108188327,41.296780523253)) ;
#14719 = CARTESIAN_POINT('Ctrl Pts',(25.6120653745065,-2.,41.0243112869525)) ;
#14720 = CARTESIAN_POINT('Ctrl Pts',(25.5833554552088,-1.99999999999999,40.7684056149203)) ;
#14721 = CARTESIAN_POINT('',(25.2874641728502,0.866025403784418,42.6156869548965)) ;
#14722 = CARTESIAN_POINT('',(25.2874641728502,-2.,42.6156869548965)) ;
#14723 = CARTESIAN_POINT('Ctrl Pts',(25.5833554552088,1.99999999999999,40.7684056149203)) ;
#14724 = CARTESIAN_POINT('Ctrl Pts',(25.6120653745065,2.,41.0243112869525)) ;
#14725 = CARTESIAN_POINT('Ctrl Pts',(25.6115056919801,1.94729108188327,41.296780523253)) ;
#14726 = CARTESIAN_POINT('Ctrl Pts',(25.5555962292677,1.74115309287314,41.7973978174612)) ;
#14727 = CARTESIAN_POINT('Ctrl Pts',(25.5013674810673,1.58802031554125,42.0257923757197)) ;
#14728 = CARTESIAN_POINT('Ctrl Pts',(25.3945042964362,1.26170274467391,42.3661460420789)) ;
#14729 = CARTESIAN_POINT('Ctrl Pts',(25.3360680744367,1.07434212579117,42.5095341847899)) ;
#14730 = CARTESIAN_POINT('Ctrl Pts',(25.2874641728502,0.866025403784424,42.6156869548965)) ;
#14731 = CARTESIAN_POINT('Origin',(22.1051760182835,2.,41.1586206896552)) ;
#14732 = CARTESIAN_POINT('Origin',(22.1051760182835,2.,41.1586206896552)) ;
#14733 = CARTESIAN_POINT('Origin',(22.1051760182835,-2.,41.1586206896552)) ;
#14734 = CARTESIAN_POINT('Origin',(24.8634926357996,0.,38.8366195187823)) ;
#14735 = CARTESIAN_POINT('',(25.3094527212108,-2.44929359829471E-16,42.8116817324112)) ;
#14736 = CARTESIAN_POINT('Origin',(25.0864726785052,0.,40.8241506255967)) ;
#14737 = CARTESIAN_POINT('Origin',(25.0864726785052,0.,40.8241506255967)) ;
#14738 = CARTESIAN_POINT('Origin',(24.8634926357996,0.,38.8366195187823)) ;
#14739 = CARTESIAN_POINT('Origin',(25.0864726785052,0.,40.8241506255967)) ;
#14740 = CARTESIAN_POINT('Origin',(45.5775257955129,0.,38.5252704302388)) ;
#14741 = CARTESIAN_POINT('',(66.2915589552262,-2.44929359829471E-16,38.2139213416953)) ;
#14742 = CARTESIAN_POINT('Origin',(66.0685789125206,0.,36.2263902348809)) ;
#14743 = CARTESIAN_POINT('',(45.8005058382185,-2.44929359829471E-16,40.5128015370533)) ;
#14744 = CARTESIAN_POINT('Origin',(65.566873816433,0.,31.7544452445484)) ;
#14745 = CARTESIAN_POINT('',(66.5702840086083,-5.5109105961631E-16,40.6983352252134)) ;
#14746 = CARTESIAN_POINT('Origin',(66.0685789125206,0.,36.2263902348809)) ;
#14747 = CARTESIAN_POINT('Origin',(67.0623444659278,0.,36.1149002135281)) ;
#14748 = CARTESIAN_POINT('',(68.5578151154227,-5.5109105961631E-16,40.4753551825078)) ;
#14749 = CARTESIAN_POINT('Origin',(68.0561100193351,0.,36.0034101921753)) ;
#14750 = CARTESIAN_POINT('',(67.5640495620155,-5.5109105961631E-16,40.5868452038606)) ;
#14751 = CARTESIAN_POINT('Origin',(68.0561100193351,0.,36.0034101921753)) ;
#14752 = CARTESIAN_POINT('',(0.,0.,0.)) ;
#14753 = CARTESIAN_POINT('Origin',(96.,2.5,52.)) ;
#14754 = CARTESIAN_POINT('',(98.,3.,52.45)) ;
#14755 = CARTESIAN_POINT('',(98.,5.,52.45)) ;
#14756 = CARTESIAN_POINT('',(98.,2.5,52.45)) ;
#14757 = CARTESIAN_POINT('',(98.,3.,51.55)) ;
#14758 = CARTESIAN_POINT('Origin',(96.,3.,52.)) ;
#14759 = CARTESIAN_POINT('',(98.,5.,51.55)) ;
#14760 = CARTESIAN_POINT('',(98.,2.5,51.55)) ;
#14761 = CARTESIAN_POINT('Origin',(96.,5.,52.)) ;
#14762 = CARTESIAN_POINT('Origin',(95.,3.,50.)) ;
#14763 = CARTESIAN_POINT('',(98.,3.,55.)) ;
#14764 = CARTESIAN_POINT('',(98.,3.,45.)) ;
#14765 = CARTESIAN_POINT('',(92.,3.,55.)) ;
#14766 = CARTESIAN_POINT('',(98.,3.,55.)) ;
#14767 = CARTESIAN_POINT('',(92.,3.,47.)) ;
#14768 = CARTESIAN_POINT('',(92.,3.,55.)) ;
#14769 = CARTESIAN_POINT('',(96.1041019662497,3.,47.)) ;
#14770 = CARTESIAN_POINT('',(93.875,3.,47.)) ;
#14771 = CARTESIAN_POINT('',(96.75,3.,46.5)) ;
#14772 = CARTESIAN_POINT('Ctrl Pts',(96.75,3.,46.5)) ;
#14773 = CARTESIAN_POINT('Ctrl Pts',(96.4100536664472,3.,46.7719570668423)) ;
#14774 = CARTESIAN_POINT('Ctrl Pts',(96.1041019662497,3.,47.)) ;
#14775 = CARTESIAN_POINT('',(96.75,3.,45.)) ;
#14776 = CARTESIAN_POINT('',(96.75,3.,41.25)) ;
#14777 = CARTESIAN_POINT('',(98.,3.,45.)) ;
#14778 = CARTESIAN_POINT('',(92.,3.,45.)) ;
#14779 = CARTESIAN_POINT('',(98.,3.,45.)) ;
#14780 = CARTESIAN_POINT('Origin',(98.,3.,55.)) ;
#14781 = CARTESIAN_POINT('',(98.,5.,55.)) ;
#14782 = CARTESIAN_POINT('',(98.,5.,45.)) ;
#14783 = CARTESIAN_POINT('',(98.,3.,55.)) ;
#14784 = CARTESIAN_POINT('Origin',(98.,3.,55.)) ;
#14785 = CARTESIAN_POINT('',(98.,5.,45.)) ;
#14786 = CARTESIAN_POINT('',(98.,3.,45.)) ;
#14787 = CARTESIAN_POINT('',(98.,5.,45.)) ;
#14788 = CARTESIAN_POINT('Origin',(98.,3.,45.)) ;
#14789 = CARTESIAN_POINT('',(92.,4.9434299833213,45.)) ;
#14790 = CARTESIAN_POINT('',(92.75,5.,45.)) ;
#14791 = CARTESIAN_POINT('Origin',(92.75,0.,45.)) ;
#14792 = CARTESIAN_POINT('',(92.,5.,45.)) ;
#14793 = CARTESIAN_POINT('',(92.,3.,45.)) ;
#14794 = CARTESIAN_POINT('',(92.,5.,45.)) ;
#14795 = CARTESIAN_POINT('Origin',(98.,3.,45.)) ;
#14796 = CARTESIAN_POINT('Origin',(92.75,0.,45.)) ;
#14797 = CARTESIAN_POINT('',(92.,5.,45.)) ;
#14798 = CARTESIAN_POINT('Origin',(92.,3.,45.)) ;
#14799 = CARTESIAN_POINT('',(92.,4.4370598373247,47.)) ;
#14800 = CARTESIAN_POINT('',(92.,1.5,47.)) ;
#14801 = CARTESIAN_POINT('',(92.,5.,55.)) ;
#14802 = CARTESIAN_POINT('',(92.,3.,55.)) ;
#14803 = CARTESIAN_POINT('',(92.,5.,55.)) ;
#14804 = CARTESIAN_POINT('',(92.,4.9434299833213,46.5)) ;
#14805 = CARTESIAN_POINT('',(92.,4.9434299833213,41.25)) ;
#14806 = CARTESIAN_POINT('Ctrl Pts',(92.,4.43705983732471,47.)) ;
#14807 = CARTESIAN_POINT('Ctrl Pts',(92.,4.67691938017707,46.7634953012913)) ;
#14808 = CARTESIAN_POINT('Ctrl Pts',(92.,4.9434299833213,46.5)) ;
#14809 = CARTESIAN_POINT('Origin',(92.,3.,55.)) ;
#14810 = CARTESIAN_POINT('',(98.,5.,55.)) ;
#14811 = CARTESIAN_POINT('Origin',(95.,5.,50.)) ;
#14812 = CARTESIAN_POINT('Origin',(92.75,0.,47.)) ;
#14813 = CARTESIAN_POINT('Origin',(92.75,0.,47.)) ;
#14814 = CARTESIAN_POINT('Origin',(92.75,0.,46.75)) ;
#14815 = CARTESIAN_POINT('',(87.75,-6.12323399573677E-16,46.5)) ;
#14816 = CARTESIAN_POINT('Origin',(92.75,0.,46.5)) ;
#14817 = CARTESIAN_POINT('Origin',(92.75,0.,46.5)) ;
#14818 = CARTESIAN_POINT('Origin',(97.75,0.,36.)) ;
#14819 = CARTESIAN_POINT('',(95.25,4.33012701892219,36.)) ;
#14820 = CARTESIAN_POINT('',(95.25,-4.33012701892219,36.)) ;
#14821 = CARTESIAN_POINT('',(95.25,-4.,36.)) ;
#14822 = CARTESIAN_POINT('Origin',(92.75,0.,36.)) ;
#14823 = CARTESIAN_POINT('Origin',(92.75,0.,41.25)) ;
#14824 = CARTESIAN_POINT('',(87.75,-6.12323399573677E-16,37.)) ;
#14825 = CARTESIAN_POINT('',(87.75,-6.12323399573677E-16,41.25)) ;
#14826 = CARTESIAN_POINT('',(95.25,-4.33012701892219,37.)) ;
#14827 = CARTESIAN_POINT('Origin',(92.75,0.,37.)) ;
#14828 = CARTESIAN_POINT('',(95.25,-4.33012701892219,41.25)) ;
#14829 = CARTESIAN_POINT('',(95.25,4.33012701892219,37.)) ;
#14830 = CARTESIAN_POINT('',(95.25,4.33012701892219,41.25)) ;
#14831 = CARTESIAN_POINT('Origin',(92.75,0.,37.)) ;
#14832 = CARTESIAN_POINT('Origin',(91.25,0.,37.)) ;
#14833 = CARTESIAN_POINT('',(95.25,8.,37.)) ;
#14834 = CARTESIAN_POINT('',(95.25,-8.,37.)) ;
#14835 = CARTESIAN_POINT('',(87.25,8.,37.)) ;
#14836 = CARTESIAN_POINT('',(95.25,8.,37.)) ;
#14837 = CARTESIAN_POINT('',(87.25,-8.,37.)) ;
#14838 = CARTESIAN_POINT('',(87.25,8.,37.)) ;
#14839 = CARTESIAN_POINT('',(95.25,-8.,37.)) ;
#14840 = CARTESIAN_POINT('',(87.25,-8.,37.)) ;
#14841 = CARTESIAN_POINT('',(95.25,-8.,37.)) ;
#14842 = CARTESIAN_POINT('Origin',(95.25,8.,29.1)) ;
#14843 = CARTESIAN_POINT('',(95.25,8.,29.1)) ;
#14844 = CARTESIAN_POINT('',(87.25,8.,29.1)) ;
#14845 = CARTESIAN_POINT('',(95.25,8.,29.1)) ;
#14846 = CARTESIAN_POINT('',(87.25,8.,29.1)) ;
#14847 = CARTESIAN_POINT('',(95.25,8.,29.1)) ;
#14848 = CARTESIAN_POINT('Origin',(95.25,-8.,29.1)) ;
#14849 = CARTESIAN_POINT('',(95.25,-8.,29.1)) ;
#14850 = CARTESIAN_POINT('',(95.25,-8.,29.1)) ;
#14851 = CARTESIAN_POINT('',(95.25,-8.,29.1)) ;
#14852 = CARTESIAN_POINT('Origin',(87.25,-8.,29.1)) ;
#14853 = CARTESIAN_POINT('',(87.25,-8.,29.1)) ;
#14854 = CARTESIAN_POINT('',(87.25,-8.,29.1)) ;
#14855 = CARTESIAN_POINT('',(87.25,-8.,29.1)) ;
#14856 = CARTESIAN_POINT('Origin',(87.25,8.,29.1)) ;
#14857 = CARTESIAN_POINT('',(87.25,8.,29.1)) ;
#14858 = CARTESIAN_POINT('Origin',(91.25,0.,29.1)) ;
#14859 = CARTESIAN_POINT('',(0.,0.,0.)) ;
#14860 = CARTESIAN_POINT('Origin',(112.,19.,33.5)) ;
#14861 = CARTESIAN_POINT('',(112.,19.,33.5)) ;
#14862 = CARTESIAN_POINT('',(100.,19.,33.5)) ;
#14863 = CARTESIAN_POINT('',(112.,19.,33.5)) ;
#14864 = CARTESIAN_POINT('',(100.,19.,36.)) ;
#14865 = CARTESIAN_POINT('',(100.,19.,33.5)) ;
#14866 = CARTESIAN_POINT('',(112.,19.,36.)) ;
#14867 = CARTESIAN_POINT('',(112.,19.,36.)) ;
#14868 = CARTESIAN_POINT('',(112.,19.,33.5)) ;
#14869 = CARTESIAN_POINT('Origin',(112.,5.1,33.5)) ;
#14870 = CARTESIAN_POINT('',(112.,5.1,33.5)) ;
#14871 = CARTESIAN_POINT('',(112.,5.1,33.5)) ;
#14872 = CARTESIAN_POINT('',(112.,5.1,36.)) ;
#14873 = CARTESIAN_POINT('',(112.,5.1,36.)) ;
#14874 = CARTESIAN_POINT('',(112.,5.1,33.5)) ;
#14875 = CARTESIAN_POINT('Origin',(100.,19.,33.5)) ;
#14876 = CARTESIAN_POINT('',(100.,5.1,33.5)) ;
#14877 = CARTESIAN_POINT('',(100.,19.,33.5)) ;
#14878 = CARTESIAN_POINT('',(100.,5.1,36.)) ;
#14879 = CARTESIAN_POINT('',(100.,5.1,33.5)) ;
#14880 = CARTESIAN_POINT('',(100.,19.,36.)) ;
#14881 = CARTESIAN_POINT('Origin',(106.,12.05,36.)) ;
#14882 = CARTESIAN_POINT('',(108.2,5.1,36.)) ;
#14883 = CARTESIAN_POINT('',(108.2,7.1,36.)) ;
#14884 = CARTESIAN_POINT('',(108.2,5.1,36.)) ;
#14885 = CARTESIAN_POINT('',(100.,5.1,36.)) ;
#14886 = CARTESIAN_POINT('',(103.405655188684,5.1,36.)) ;
#14887 = CARTESIAN_POINT('',(100.,5.1,36.)) ;
#14888 = CARTESIAN_POINT('',(103.405655188684,7.1,36.)) ;
#14889 = CARTESIAN_POINT('',(103.405655188684,8.575,36.)) ;
#14890 = CARTESIAN_POINT('',(103.5,7.1,36.)) ;
#14891 = CARTESIAN_POINT('Origin',(106.,12.05,33.5)) ;
#14892 = CARTESIAN_POINT('',(100.,5.1,33.5)) ;
#14893 = CARTESIAN_POINT('Origin',(101.,7.1,44.)) ;
#14894 = CARTESIAN_POINT('',(94.1344037311888,7.1,50.834002331993)) ;
#14895 = CARTESIAN_POINT('',(104.134403731189,7.1,34.834002331993)) ;
#14896 = CARTESIAN_POINT('',(97.8655962688112,7.1,53.165997668007)) ;
#14897 = CARTESIAN_POINT('Origin',(96.,7.1,52.)) ;
#14898 = CARTESIAN_POINT('',(107.865596268811,7.1,37.165997668007)) ;
#14899 = CARTESIAN_POINT('',(97.8655962688112,7.1,53.165997668007)) ;
#14900 = CARTESIAN_POINT('Origin',(106.,7.1,36.)) ;
#14901 = CARTESIAN_POINT('',(93.95,7.1,52.)) ;
#14902 = CARTESIAN_POINT('Origin',(96.,7.1,52.)) ;
#14903 = CARTESIAN_POINT('Origin',(104.134403731189,5.1,34.834002331993)) ;
#14904 = CARTESIAN_POINT('',(94.1344037311888,5.1,50.834002331993)) ;
#14905 = CARTESIAN_POINT('',(104.134403731189,5.1,34.834002331993)) ;
#14906 = CARTESIAN_POINT('',(94.1344037311888,5.1,50.834002331993)) ;
#14907 = CARTESIAN_POINT('Origin',(96.,5.1,52.)) ;
#14908 = CARTESIAN_POINT('',(93.95,5.1,52.)) ;
#14909 = CARTESIAN_POINT('',(93.95,5.1,52.)) ;
#14910 = CARTESIAN_POINT('Origin',(96.,5.1,52.)) ;
#14911 = CARTESIAN_POINT('Origin',(106.,5.1,36.)) ;
#14912 = CARTESIAN_POINT('',(107.865596268811,5.1,37.165997668007)) ;
#14913 = CARTESIAN_POINT('',(107.865596268811,5.1,37.165997668007)) ;
#14914 = CARTESIAN_POINT('Origin',(106.,5.1,36.)) ;
#14915 = CARTESIAN_POINT('Origin',(97.8655962688112,5.1,53.165997668007)) ;
#14916 = CARTESIAN_POINT('',(97.8655962688112,5.1,53.165997668007)) ;
#14917 = CARTESIAN_POINT('',(97.8655962688112,5.1,53.165997668007)) ;
#14918 = CARTESIAN_POINT('',(97.8655962688112,5.1,53.165997668007)) ;
#14919 = CARTESIAN_POINT('Origin',(96.,5.1,52.)) ;
#14920 = CARTESIAN_POINT('Origin',(96.,5.1,52.)) ;
#14921 = CARTESIAN_POINT('Origin',(101.,5.1,44.)) ;
#14922 = CARTESIAN_POINT('',(0.,0.,0.)) ;
#14923 = CARTESIAN_POINT('Origin',(87.1,-45.,50.)) ;
#14924 = CARTESIAN_POINT('',(87.1,-45.,48.95)) ;
#14925 = CARTESIAN_POINT('',(87.1,-45.,51.05)) ;
#14926 = CARTESIAN_POINT('Ctrl Pts',(87.1,-45.,48.95)) ;
#14927 = CARTESIAN_POINT('Ctrl Pts',(87.1,-45.1331635999932,48.95)) ;
#14928 = CARTESIAN_POINT('Ctrl Pts',(87.0897621937364,-45.2743704641551,48.9768675662366)) ;
#14929 = CARTESIAN_POINT('Ctrl Pts',(87.0528075475038,-45.5327272469311,49.0844232537265)) ;
#14930 = CARTESIAN_POINT('Ctrl Pts',(87.0265476839081,-45.6499697400254,49.1650454995336)) ;
#14931 = CARTESIAN_POINT('Ctrl Pts',(86.9766154867118,-45.835020200063,49.3500959595712)) ;
#14932 = CARTESIAN_POINT('Ctrl Pts',(86.9495293742091,-45.9155922350857,49.4673129257906)) ;
#14933 = CARTESIAN_POINT('Ctrl Pts',(86.9106416723388,-46.0231099988203,49.725572678198)) ;
#14934 = CARTESIAN_POINT('Ctrl Pts',(86.8995282598983,-46.05,49.8667418106495)) ;
#14935 = CARTESIAN_POINT('Ctrl Pts',(86.8995282598983,-46.05,50.1332581893505)) ;
#14936 = CARTESIAN_POINT('Ctrl Pts',(86.9106416723388,-46.0231099988203,50.274427321802)) ;
#14937 = CARTESIAN_POINT('Ctrl Pts',(86.9495293742091,-45.9155922350857,50.5326870742094)) ;
#14938 = CARTESIAN_POINT('Ctrl Pts',(86.9766154867118,-45.835020200063,50.6499040404288)) ;
#14939 = CARTESIAN_POINT('Ctrl Pts',(87.0265476839081,-45.6499697400254,50.8349545004664)) ;
#14940 = CARTESIAN_POINT('Ctrl Pts',(87.0528075475038,-45.5327272469311,50.9155767462735)) ;
#14941 = CARTESIAN_POINT('Ctrl Pts',(87.0897621937364,-45.2743704641551,51.0231324337635)) ;
#14942 = CARTESIAN_POINT('Ctrl Pts',(87.1,-45.1331635999932,51.05)) ;
#14943 = CARTESIAN_POINT('Ctrl Pts',(87.1,-45.,51.05)) ;
#14944 = CARTESIAN_POINT('Ctrl Pts',(87.1,-45.,51.05)) ;
#14945 = CARTESIAN_POINT('Ctrl Pts',(87.1,-44.8668364000068,51.05)) ;
#14946 = CARTESIAN_POINT('Ctrl Pts',(87.0897621937364,-44.7256295358449,51.0231324337635)) ;
#14947 = CARTESIAN_POINT('Ctrl Pts',(87.0528075475038,-44.4672727530689,50.9155767462735)) ;
#14948 = CARTESIAN_POINT('Ctrl Pts',(87.0265476839081,-44.3500302599746,50.8349545004664)) ;
#14949 = CARTESIAN_POINT('Ctrl Pts',(86.9766154867118,-44.164979799937,50.6499040404288)) ;
#14950 = CARTESIAN_POINT('Ctrl Pts',(86.9495293742091,-44.0844077649143,50.5326870742094)) ;
#14951 = CARTESIAN_POINT('Ctrl Pts',(86.9106416723388,-43.9768900011798,50.274427321802)) ;
#14952 = CARTESIAN_POINT('Ctrl Pts',(86.8995282598984,-43.95,50.1332581893505)) ;
#14953 = CARTESIAN_POINT('Ctrl Pts',(86.8995282598984,-43.95,50.)) ;
#14954 = CARTESIAN_POINT('Ctrl Pts',(86.8995282598984,-43.95,49.8667418106495)) ;
#14955 = CARTESIAN_POINT('Ctrl Pts',(86.9106416723388,-43.9768900011797,49.725572678198)) ;
#14956 = CARTESIAN_POINT('Ctrl Pts',(86.9495293742091,-44.0844077649143,49.4673129257906)) ;
#14957 = CARTESIAN_POINT('Ctrl Pts',(86.9766154867118,-44.164979799937,49.3500959595712)) ;
#14958 = CARTESIAN_POINT('Ctrl Pts',(87.0265476839081,-44.3500302599746,49.1650454995336)) ;
#14959 = CARTESIAN_POINT('Ctrl Pts',(87.0528075475038,-44.4672727530689,49.0844232537265)) ;
#14960 = CARTESIAN_POINT('Ctrl Pts',(87.0897621937364,-44.7256295358449,48.9768675662366)) ;
#14961 = CARTESIAN_POINT('Ctrl Pts',(87.1,-44.8668364000068,48.95)) ;
#14962 = CARTESIAN_POINT('Ctrl Pts',(87.1,-45.,48.95)) ;
#14963 = CARTESIAN_POINT('',(81.4,-45.,51.05)) ;
#14964 = CARTESIAN_POINT('',(87.1,-45.,51.05)) ;
#14965 = CARTESIAN_POINT('',(81.4,-45.,48.95)) ;
#14966 = CARTESIAN_POINT('Ctrl Pts',(81.4,-45.,48.95)) ;
#14967 = CARTESIAN_POINT('Ctrl Pts',(81.4,-44.8668364000068,48.95)) ;
#14968 = CARTESIAN_POINT('Ctrl Pts',(81.4102378062637,-44.7256295358449,48.9768675662366)) ;
#14969 = CARTESIAN_POINT('Ctrl Pts',(81.4471924524962,-44.4672727530689,49.0844232537265)) ;
#14970 = CARTESIAN_POINT('Ctrl Pts',(81.4734523160919,-44.3500302599746,49.1650454995336)) ;
#14971 = CARTESIAN_POINT('Ctrl Pts',(81.5233845132882,-44.164979799937,49.3500959595712)) ;
#14972 = CARTESIAN_POINT('Ctrl Pts',(81.5504706257909,-44.0844077649143,49.4673129257906)) ;
#14973 = CARTESIAN_POINT('Ctrl Pts',(81.5893583276612,-43.9768900011797,49.725572678198)) ;
#14974 = CARTESIAN_POINT('Ctrl Pts',(81.6004717401017,-43.95,49.8667418106495)) ;
#14975 = CARTESIAN_POINT('Ctrl Pts',(81.6004717401017,-43.95,50.)) ;
#14976 = CARTESIAN_POINT('Ctrl Pts',(81.6004717401017,-43.95,50.1332581893505)) ;
#14977 = CARTESIAN_POINT('Ctrl Pts',(81.5893583276612,-43.9768900011798,50.274427321802)) ;
#14978 = CARTESIAN_POINT('Ctrl Pts',(81.5504706257909,-44.0844077649143,50.5326870742094)) ;
#14979 = CARTESIAN_POINT('Ctrl Pts',(81.5233845132882,-44.164979799937,50.6499040404288)) ;
#14980 = CARTESIAN_POINT('Ctrl Pts',(81.4734523160919,-44.3500302599746,50.8349545004664)) ;
#14981 = CARTESIAN_POINT('Ctrl Pts',(81.4471924524962,-44.4672727530689,50.9155767462735)) ;
#14982 = CARTESIAN_POINT('Ctrl Pts',(81.4102378062637,-44.7256295358449,51.0231324337635)) ;
#14983 = CARTESIAN_POINT('Ctrl Pts',(81.4,-44.8668364000068,51.05)) ;
#14984 = CARTESIAN_POINT('Ctrl Pts',(81.4,-45.,51.05)) ;
#14985 = CARTESIAN_POINT('Ctrl Pts',(81.4,-45.,51.05)) ;
#14986 = CARTESIAN_POINT('Ctrl Pts',(81.4,-45.1331635999932,51.05)) ;
#14987 = CARTESIAN_POINT('Ctrl Pts',(81.4102378062637,-45.2743704641551,51.0231324337634)) ;
#14988 = CARTESIAN_POINT('Ctrl Pts',(81.4471924524962,-45.5327272469311,50.9155767462735)) ;
#14989 = CARTESIAN_POINT('Ctrl Pts',(81.4734523160919,-45.6499697400254,50.8349545004664)) ;
#14990 = CARTESIAN_POINT('Ctrl Pts',(81.5233845132883,-45.835020200063,50.6499040404288)) ;
#14991 = CARTESIAN_POINT('Ctrl Pts',(81.5504706257909,-45.9155922350857,50.5326870742094)) ;
#14992 = CARTESIAN_POINT('Ctrl Pts',(81.5893583276612,-46.0231099988203,50.274427321802)) ;
#14993 = CARTESIAN_POINT('Ctrl Pts',(81.6004717401017,-46.05,50.1332581893505)) ;
#14994 = CARTESIAN_POINT('Ctrl Pts',(81.6004717401017,-46.05,49.8667418106495)) ;
#14995 = CARTESIAN_POINT('Ctrl Pts',(81.5893583276612,-46.0231099988203,49.725572678198)) ;
#14996 = CARTESIAN_POINT('Ctrl Pts',(81.5504706257909,-45.9155922350857,49.4673129257906)) ;
#14997 = CARTESIAN_POINT('Ctrl Pts',(81.5233845132883,-45.835020200063,49.3500959595712)) ;
#14998 = CARTESIAN_POINT('Ctrl Pts',(81.4734523160919,-45.6499697400254,49.1650454995336)) ;
#14999 = CARTESIAN_POINT('Ctrl Pts',(81.4471924524962,-45.5327272469311,49.0844232537265)) ;
#15000 = CARTESIAN_POINT('Ctrl Pts',(81.4102378062637,-45.2743704641551,48.9768675662366)) ;
#15001 = CARTESIAN_POINT('Ctrl Pts',(81.4,-45.1331635999932,48.95)) ;
#15002 = CARTESIAN_POINT('Ctrl Pts',(81.4,-45.,48.95)) ;
#15003 = CARTESIAN_POINT('Origin',(87.1,45.,50.)) ;
#15004 = CARTESIAN_POINT('',(87.1,45.,51.05)) ;
#15005 = CARTESIAN_POINT('',(87.1,45.,48.95)) ;
#15006 = CARTESIAN_POINT('Ctrl Pts',(87.1,45.,51.05)) ;
#15007 = CARTESIAN_POINT('Ctrl Pts',(87.1,45.1331635999932,51.05)) ;
#15008 = CARTESIAN_POINT('Ctrl Pts',(87.0897621937364,45.2743704641552,51.0231324337635)) ;
#15009 = CARTESIAN_POINT('Ctrl Pts',(87.0528075475038,45.5327272469311,50.9155767462735)) ;
#15010 = CARTESIAN_POINT('Ctrl Pts',(87.0265476839081,45.6499697400254,50.8349545004664)) ;
#15011 = CARTESIAN_POINT('Ctrl Pts',(86.9766154867118,45.835020200063,50.6499040404288)) ;
#15012 = CARTESIAN_POINT('Ctrl Pts',(86.9495293742091,45.9155922350857,50.5326870742094)) ;
#15013 = CARTESIAN_POINT('Ctrl Pts',(86.9106416723389,46.0231099988203,50.274427321802)) ;
#15014 = CARTESIAN_POINT('Ctrl Pts',(86.8995282598984,46.05,50.1332581893505)) ;
#15015 = CARTESIAN_POINT('Ctrl Pts',(86.8995282598984,46.05,49.8667418106495)) ;
#15016 = CARTESIAN_POINT('Ctrl Pts',(86.9106416723389,46.0231099988203,49.725572678198)) ;
#15017 = CARTESIAN_POINT('Ctrl Pts',(86.9495293742091,45.9155922350857,49.4673129257906)) ;
#15018 = CARTESIAN_POINT('Ctrl Pts',(86.9766154867118,45.835020200063,49.3500959595712)) ;
#15019 = CARTESIAN_POINT('Ctrl Pts',(87.0265476839081,45.6499697400254,49.1650454995336)) ;
#15020 = CARTESIAN_POINT('Ctrl Pts',(87.0528075475038,45.5327272469311,49.0844232537265)) ;
#15021 = CARTESIAN_POINT('Ctrl Pts',(87.0897621937364,45.2743704641552,48.9768675662365)) ;
#15022 = CARTESIAN_POINT('Ctrl Pts',(87.1,45.1331635999932,48.95)) ;
#15023 = CARTESIAN_POINT('Ctrl Pts',(87.1,45.,48.95)) ;
#15024 = CARTESIAN_POINT('',(81.4,45.,51.05)) ;
#15025 = CARTESIAN_POINT('',(87.1,45.,51.05)) ;
#15026 = CARTESIAN_POINT('',(81.4,45.,48.95)) ;
#15027 = CARTESIAN_POINT('Ctrl Pts',(81.4,45.,48.95)) ;
#15028 = CARTESIAN_POINT('Ctrl Pts',(81.4,45.1331635999932,48.95)) ;
#15029 = CARTESIAN_POINT('Ctrl Pts',(81.4102378062637,45.2743704641552,48.9768675662365)) ;
#15030 = CARTESIAN_POINT('Ctrl Pts',(81.4471924524962,45.5327272469311,49.0844232537265)) ;
#15031 = CARTESIAN_POINT('Ctrl Pts',(81.4734523160919,45.6499697400254,49.1650454995336)) ;
#15032 = CARTESIAN_POINT('Ctrl Pts',(81.5233845132882,45.835020200063,49.3500959595712)) ;
#15033 = CARTESIAN_POINT('Ctrl Pts',(81.5504706257909,45.9155922350857,49.4673129257906)) ;
#15034 = CARTESIAN_POINT('Ctrl Pts',(81.5893583276612,46.0231099988203,49.725572678198)) ;
#15035 = CARTESIAN_POINT('Ctrl Pts',(81.6004717401017,46.05,49.8667418106495)) ;
#15036 = CARTESIAN_POINT('Ctrl Pts',(81.6004717401017,46.05,50.1332581893505)) ;
#15037 = CARTESIAN_POINT('Ctrl Pts',(81.5893583276612,46.0231099988203,50.274427321802)) ;
#15038 = CARTESIAN_POINT('Ctrl Pts',(81.5504706257909,45.9155922350857,50.5326870742094)) ;
#15039 = CARTESIAN_POINT('Ctrl Pts',(81.5233845132882,45.835020200063,50.6499040404288)) ;
#15040 = CARTESIAN_POINT('Ctrl Pts',(81.4734523160919,45.6499697400254,50.8349545004664)) ;
#15041 = CARTESIAN_POINT('Ctrl Pts',(81.4471924524962,45.5327272469311,50.9155767462735)) ;
#15042 = CARTESIAN_POINT('Ctrl Pts',(81.4102378062637,45.2743704641552,51.0231324337635)) ;
#15043 = CARTESIAN_POINT('Ctrl Pts',(81.4,45.1331635999932,51.05)) ;
#15044 = CARTESIAN_POINT('Ctrl Pts',(81.4,45.,51.05)) ;
#15045 = CARTESIAN_POINT('Ctrl Pts',(81.4,45.,51.05)) ;
#15046 = CARTESIAN_POINT('Ctrl Pts',(81.4,44.8668364000068,51.05)) ;
#15047 = CARTESIAN_POINT('Ctrl Pts',(81.4102378062637,44.7256295358448,51.0231324337635)) ;
#15048 = CARTESIAN_POINT('Ctrl Pts',(81.4471924524962,44.4672727530689,50.9155767462735)) ;
#15049 = CARTESIAN_POINT('Ctrl Pts',(81.4734523160919,44.3500302599746,50.8349545004664)) ;
#15050 = CARTESIAN_POINT('Ctrl Pts',(81.5233845132882,44.164979799937,50.6499040404288)) ;
#15051 = CARTESIAN_POINT('Ctrl Pts',(81.5504706257909,44.0844077649143,50.5326870742094)) ;
#15052 = CARTESIAN_POINT('Ctrl Pts',(81.5893583276612,43.9768900011797,50.274427321802)) ;
#15053 = CARTESIAN_POINT('Ctrl Pts',(81.6004717401017,43.95,50.1332581893505)) ;
#15054 = CARTESIAN_POINT('Ctrl Pts',(81.6004717401017,43.95,50.)) ;
#15055 = CARTESIAN_POINT('Ctrl Pts',(81.6004717401017,43.95,49.8667418106495)) ;
#15056 = CARTESIAN_POINT('Ctrl Pts',(81.5893583276612,43.9768900011797,49.725572678198)) ;
#15057 = CARTESIAN_POINT('Ctrl Pts',(81.5504706257909,44.0844077649143,49.4673129257906)) ;
#15058 = CARTESIAN_POINT('Ctrl Pts',(81.5233845132882,44.164979799937,49.3500959595712)) ;
#15059 = CARTESIAN_POINT('Ctrl Pts',(81.4734523160919,44.3500302599746,49.1650454995336)) ;
#15060 = CARTESIAN_POINT('Ctrl Pts',(81.4471924524962,44.4672727530689,49.0844232537265)) ;
#15061 = CARTESIAN_POINT('Ctrl Pts',(81.4102378062637,44.7256295358448,48.9768675662365)) ;
#15062 = CARTESIAN_POINT('Ctrl Pts',(81.4,44.8668364000068,48.95)) ;
#15063 = CARTESIAN_POINT('Ctrl Pts',(81.4,45.,48.95)) ;
#15064 = CARTESIAN_POINT('Ctrl Pts',(87.1,45.,48.95)) ;
#15065 = CARTESIAN_POINT('Ctrl Pts',(87.1,44.8668364000068,48.95)) ;
#15066 = CARTESIAN_POINT('Ctrl Pts',(87.0897621937364,44.7256295358448,48.9768675662365)) ;
#15067 = CARTESIAN_POINT('Ctrl Pts',(87.0528075475038,44.4672727530689,49.0844232537265)) ;
#15068 = CARTESIAN_POINT('Ctrl Pts',(87.0265476839081,44.3500302599746,49.1650454995336)) ;
#15069 = CARTESIAN_POINT('Ctrl Pts',(86.9766154867118,44.164979799937,49.3500959595712)) ;
#15070 = CARTESIAN_POINT('Ctrl Pts',(86.9495293742091,44.0844077649143,49.4673129257906)) ;
#15071 = CARTESIAN_POINT('Ctrl Pts',(86.9106416723389,43.9768900011797,49.725572678198)) ;
#15072 = CARTESIAN_POINT('Ctrl Pts',(86.8995282598984,43.95,49.8667418106495)) ;
#15073 = CARTESIAN_POINT('Ctrl Pts',(86.8995282598984,43.95,50.)) ;
#15074 = CARTESIAN_POINT('Ctrl Pts',(86.8995282598984,43.95,50.1332581893505)) ;
#15075 = CARTESIAN_POINT('Ctrl Pts',(86.9106416723389,43.9768900011797,50.274427321802)) ;
#15076 = CARTESIAN_POINT('Ctrl Pts',(86.9495293742091,44.0844077649143,50.5326870742094)) ;
#15077 = CARTESIAN_POINT('Ctrl Pts',(86.9766154867118,44.164979799937,50.6499040404288)) ;
#15078 = CARTESIAN_POINT('Ctrl Pts',(87.0265476839081,44.3500302599746,50.8349545004664)) ;
#15079 = CARTESIAN_POINT('Ctrl Pts',(87.0528075475038,44.4672727530689,50.9155767462735)) ;
#15080 = CARTESIAN_POINT('Ctrl Pts',(87.0897621937364,44.7256295358448,51.0231324337635)) ;
#15081 = CARTESIAN_POINT('Ctrl Pts',(87.1,44.8668364000068,51.05)) ;
#15082 = CARTESIAN_POINT('Ctrl Pts',(87.1,45.,51.05)) ;
#15083 = CARTESIAN_POINT('Origin',(90.25,42.5,160.)) ;
#15084 = CARTESIAN_POINT('',(88.2,43.,160.)) ;
#15085 = CARTESIAN_POINT('Origin',(90.25,43.,160.)) ;
#15086 = CARTESIAN_POINT('',(88.2,47.,160.)) ;
#15087 = CARTESIAN_POINT('',(88.2,42.5,160.)) ;
#15088 = CARTESIAN_POINT('Origin',(90.25,47.,160.)) ;
#15089 = CARTESIAN_POINT('Origin',(89.5,45.,163.)) ;
#15090 = CARTESIAN_POINT('',(86.5,43.2507144315464,163.)) ;
#15091 = CARTESIAN_POINT('',(86.5,46.7492855684536,163.)) ;
#15092 = CARTESIAN_POINT('Origin',(84.25,45.,163.)) ;
#15093 = CARTESIAN_POINT('',(86.5,43.,163.)) ;
#15094 = CARTESIAN_POINT('',(86.5,47.,163.)) ;
#15095 = CARTESIAN_POINT('',(92.5,43.,163.)) ;
#15096 = CARTESIAN_POINT('',(86.5,43.,163.)) ;
#15097 = CARTESIAN_POINT('',(92.5,47.,163.)) ;
#15098 = CARTESIAN_POINT('',(92.5,43.,163.)) ;
#15099 = CARTESIAN_POINT('',(86.5,47.,163.)) ;
#15100 = CARTESIAN_POINT('',(92.5,47.,163.)) ;
#15101 = CARTESIAN_POINT('',(86.5,47.,163.)) ;
#15102 = CARTESIAN_POINT('Origin',(86.5,47.,157.)) ;
#15103 = CARTESIAN_POINT('',(86.5,43.2507144315464,157.)) ;
#15104 = CARTESIAN_POINT('',(86.5,43.2507144315464,41.)) ;
#15105 = CARTESIAN_POINT('',(86.5,43.,157.)) ;
#15106 = CARTESIAN_POINT('',(86.5,47.,157.)) ;
#15107 = CARTESIAN_POINT('',(86.5,43.,157.)) ;
#15108 = CARTESIAN_POINT('Origin',(92.5,47.,157.)) ;
#15109 = CARTESIAN_POINT('',(92.5,47.,157.)) ;
#15110 = CARTESIAN_POINT('',(86.5,47.,157.)) ;
#15111 = CARTESIAN_POINT('',(92.5,47.,157.)) ;
#15112 = CARTESIAN_POINT('',(86.5,47.,157.)) ;
#15113 = CARTESIAN_POINT('',(92.5,47.,157.)) ;
#15114 = CARTESIAN_POINT('Origin',(92.5,43.,157.)) ;
#15115 = CARTESIAN_POINT('',(92.5,43.,157.)) ;
#15116 = CARTESIAN_POINT('',(92.5,43.,157.)) ;
#15117 = CARTESIAN_POINT('',(92.5,43.,157.)) ;
#15118 = CARTESIAN_POINT('Origin',(86.5,43.,157.)) ;
#15119 = CARTESIAN_POINT('',(86.5,43.,157.)) ;
#15120 = CARTESIAN_POINT('Origin',(86.5,47.,157.)) ;
#15121 = CARTESIAN_POINT('',(86.5,46.7492855684536,157.)) ;
#15122 = CARTESIAN_POINT('',(86.5,46.7492855684536,41.)) ;
#15123 = CARTESIAN_POINT('',(86.5,47.,157.)) ;
#15124 = CARTESIAN_POINT('Origin',(89.5,45.,157.)) ;
#15125 = CARTESIAN_POINT('Origin',(84.25,45.,157.)) ;
#15126 = CARTESIAN_POINT('Origin',(84.25,-45.,170.)) ;
#15127 = CARTESIAN_POINT('',(81.4,-45.,41.)) ;
#15128 = CARTESIAN_POINT('Origin',(84.25,-45.,41.)) ;
#15129 = CARTESIAN_POINT('',(81.4,-45.,170.)) ;
#15130 = CARTESIAN_POINT('',(81.4,-45.,170.)) ;
#15131 = CARTESIAN_POINT('',(81.4,-45.,170.)) ;
#15132 = CARTESIAN_POINT('',(84.25,-42.15,170.)) ;
#15133 = CARTESIAN_POINT('Origin',(84.25,-45.,170.)) ;
#15134 = CARTESIAN_POINT('Origin',(84.25,-45.,170.)) ;
#15135 = CARTESIAN_POINT('Origin',(84.25,-35.,170.)) ;
#15136 = CARTESIAN_POINT('',(84.25,-35.,177.15)) ;
#15137 = CARTESIAN_POINT('Origin',(84.25,-35.,170.)) ;
#15138 = CARTESIAN_POINT('',(81.4,-35.,180.)) ;
#15139 = CARTESIAN_POINT('Origin',(84.25,-35.,180.)) ;
#15140 = CARTESIAN_POINT('Origin',(84.25,-35.,180.)) ;
#15141 = CARTESIAN_POINT('Origin',(84.25,35.,180.)) ;
#15142 = CARTESIAN_POINT('',(81.4,35.,180.)) ;
#15143 = CARTESIAN_POINT('',(81.4,35.,180.)) ;
#15144 = CARTESIAN_POINT('',(84.25,35.,177.15)) ;
#15145 = CARTESIAN_POINT('Origin',(84.25,35.,180.)) ;
#15146 = CARTESIAN_POINT('Origin',(84.25,35.,180.)) ;
#15147 = CARTESIAN_POINT('Origin',(84.25,35.,170.)) ;
#15148 = CARTESIAN_POINT('',(84.25,42.15,170.)) ;
#15149 = CARTESIAN_POINT('Origin',(84.25,35.,170.)) ;
#15150 = CARTESIAN_POINT('',(81.4,45.,170.)) ;
#15151 = CARTESIAN_POINT('Origin',(84.25,45.,170.)) ;
#15152 = CARTESIAN_POINT('Origin',(84.25,45.,170.)) ;
#15153 = CARTESIAN_POINT('Origin',(84.25,45.,41.)) ;
#15154 = CARTESIAN_POINT('',(81.4,45.,41.)) ;
#15155 = CARTESIAN_POINT('',(81.4,45.,41.)) ;
#15156 = CARTESIAN_POINT('',(81.4,45.,41.)) ;
#15157 = CARTESIAN_POINT('Origin',(84.25,45.,41.)) ;
#15158 = CARTESIAN_POINT('Origin',(84.25,-45.,41.)) ;
#15159 = CARTESIAN_POINT('Origin',(84.25,45.,41.)) ;
#15160 = CARTESIAN_POINT('',(0.,0.,0.)) ;
#15161 = CARTESIAN_POINT('Origin',(90.25,47.1,160.)) ;
#15162 = CARTESIAN_POINT('',(88.2,48.1,160.)) ;
#15163 = CARTESIAN_POINT('Origin',(90.25,48.1,160.)) ;
#15164 = CARTESIAN_POINT('',(88.2,47.1,160.)) ;
#15165 = CARTESIAN_POINT('',(88.2,47.1,160.)) ;
#15166 = CARTESIAN_POINT('Origin',(90.25,47.1,160.)) ;
#15167 = CARTESIAN_POINT('Origin',(95.1682075596715,47.1,175.627339325681)) ;
#15168 = CARTESIAN_POINT('',(95.1682075596715,47.1,175.627339325681)) ;
#15169 = CARTESIAN_POINT('',(92.4182075596715,47.1,159.627339325681)) ;
#15170 = CARTESIAN_POINT('',(95.1682075596715,47.1,175.627339325681)) ;
#15171 = CARTESIAN_POINT('',(92.4182075596715,48.1,159.627339325681)) ;
#15172 = CARTESIAN_POINT('',(92.4182075596715,47.1,159.627339325681)) ;
#15173 = CARTESIAN_POINT('',(95.1682075596715,48.1,175.627339325681)) ;
#15174 = CARTESIAN_POINT('',(95.1682075596715,48.1,175.627339325681)) ;
#15175 = CARTESIAN_POINT('',(95.1682075596715,47.1,175.627339325681)) ;
#15176 = CARTESIAN_POINT('Origin',(93.,47.1,176.)) ;
#15177 = CARTESIAN_POINT('',(90.8317924403285,47.1,176.372660674319)) ;
#15178 = CARTESIAN_POINT('Origin',(93.,47.1,176.)) ;
#15179 = CARTESIAN_POINT('',(90.8317924403285,48.1,176.372660674319)) ;
#15180 = CARTESIAN_POINT('Origin',(93.,48.1,176.)) ;
#15181 = CARTESIAN_POINT('',(90.8317924403285,47.1,176.372660674319)) ;
#15182 = CARTESIAN_POINT('Origin',(88.0817924403285,47.1,160.372660674319)) ;
#15183 = CARTESIAN_POINT('',(88.0817924403285,47.1,160.372660674319)) ;
#15184 = CARTESIAN_POINT('',(88.0817924403285,47.1,160.372660674319)) ;
#15185 = CARTESIAN_POINT('',(88.0817924403285,48.1,160.372660674319)) ;
#15186 = CARTESIAN_POINT('',(88.0817924403285,48.1,160.372660674319)) ;
#15187 = CARTESIAN_POINT('',(88.0817924403285,47.1,160.372660674319)) ;
#15188 = CARTESIAN_POINT('Origin',(90.25,47.1,160.)) ;
#15189 = CARTESIAN_POINT('Origin',(90.25,47.1,160.)) ;
#15190 = CARTESIAN_POINT('Origin',(90.25,48.1,160.)) ;
#15191 = CARTESIAN_POINT('Origin',(91.625,48.1,168.)) ;
#15192 = CARTESIAN_POINT('Origin',(91.625,47.1,168.)) ;
#15193 = CARTESIAN_POINT('',(0.,0.,0.)) ;
#15194 = CARTESIAN_POINT('Origin',(74.8,56.1,35.)) ;
#15195 = CARTESIAN_POINT('',(69.2,56.1,35.)) ;
#15196 = CARTESIAN_POINT('Origin',(72.,56.1,35.)) ;
#15197 = CARTESIAN_POINT('Origin',(72.,56.,35.)) ;
#15198 = CARTESIAN_POINT('',(69.,55.9,35.)) ;
#15199 = CARTESIAN_POINT('Origin',(72.,55.9,35.)) ;
#15200 = CARTESIAN_POINT('',(69.1,56.,35.)) ;
#15201 = CARTESIAN_POINT('Origin',(72.,55.6,35.)) ;
#15202 = CARTESIAN_POINT('',(69.,55.3,35.)) ;
#15203 = CARTESIAN_POINT('Origin',(72.,55.3,35.)) ;
#15204 = CARTESIAN_POINT('',(69.,55.6,35.)) ;
#15205 = CARTESIAN_POINT('Origin',(74.,55.3,35.)) ;
#15206 = CARTESIAN_POINT('',(70.,55.3,35.)) ;
#15207 = CARTESIAN_POINT('Origin',(72.,55.3,35.)) ;
#15208 = CARTESIAN_POINT('Origin',(72.,50.05,35.)) ;
#15209 = CARTESIAN_POINT('',(70.,44.8,35.)) ;
#15210 = CARTESIAN_POINT('Origin',(72.,44.8,35.)) ;
#15211 = CARTESIAN_POINT('',(70.,50.05,35.)) ;
#15212 = CARTESIAN_POINT('Origin',(73.6,44.8,35.)) ;
#15213 = CARTESIAN_POINT('',(70.4,44.8,35.)) ;
#15214 = CARTESIAN_POINT('Origin',(72.,44.8,35.)) ;
#15215 = CARTESIAN_POINT('Origin',(72.,44.5,35.)) ;
#15216 = CARTESIAN_POINT('',(70.4,44.2,35.)) ;
#15217 = CARTESIAN_POINT('Origin',(72.,44.2,35.)) ;
#15218 = CARTESIAN_POINT('',(70.4,44.5,35.)) ;
#15219 = CARTESIAN_POINT('Origin',(74.,44.2,35.)) ;
#15220 = CARTESIAN_POINT('',(70.,44.2,35.)) ;
#15221 = CARTESIAN_POINT('Origin',(72.,44.2,35.)) ;
#15222 = CARTESIAN_POINT('Origin',(72.,44.175,35.)) ;
#15223 = CARTESIAN_POINT('',(70.,44.15,35.)) ;
#15224 = CARTESIAN_POINT('Origin',(72.,44.15,35.)) ;
#15225 = CARTESIAN_POINT('',(70.,44.175,35.)) ;
#15226 = CARTESIAN_POINT('Origin',(72.,44.025,35.)) ;
#15227 = CARTESIAN_POINT('',(70.25,43.9,35.)) ;
#15228 = CARTESIAN_POINT('Origin',(72.,43.9,35.)) ;
#15229 = CARTESIAN_POINT('',(70.125,44.025,35.)) ;
#15230 = CARTESIAN_POINT('Origin',(72.,43.9,35.)) ;
#15231 = CARTESIAN_POINT('',(0.,0.,0.)) ;
#15232 = CARTESIAN_POINT('Origin',(70.4,44.1,34.)) ;
#15233 = CARTESIAN_POINT('',(73.2489995996797,44.2,34.)) ;
#15234 = CARTESIAN_POINT('',(73.6,44.2,34.)) ;
#15235 = CARTESIAN_POINT('',(72.,44.2,34.)) ;
#15236 = CARTESIAN_POINT('',(73.2489995996797,44.8,34.)) ;
#15237 = CARTESIAN_POINT('',(73.2489995996797,44.5,34.)) ;
#15238 = CARTESIAN_POINT('',(73.6,44.8,34.)) ;
#15239 = CARTESIAN_POINT('',(73.025,44.8,34.)) ;
#15240 = CARTESIAN_POINT('',(73.6,44.1,34.)) ;
#15241 = CARTESIAN_POINT('Origin',(70.4,44.1,34.)) ;
#15242 = CARTESIAN_POINT('',(70.4,44.2,34.)) ;
#15243 = CARTESIAN_POINT('',(70.7510004003203,44.2,34.)) ;
#15244 = CARTESIAN_POINT('',(72.,44.2,34.)) ;
#15245 = CARTESIAN_POINT('',(70.4,44.8,34.)) ;
#15246 = CARTESIAN_POINT('',(70.4,44.1,34.)) ;
#15247 = CARTESIAN_POINT('',(70.7510004003203,44.8,34.)) ;
#15248 = CARTESIAN_POINT('',(73.025,44.8,34.)) ;
#15249 = CARTESIAN_POINT('',(70.7510004003203,44.5,34.)) ;
#15250 = CARTESIAN_POINT('Origin',(73.6,44.1,34.)) ;
#15251 = CARTESIAN_POINT('',(73.6,44.2,31.7193750595351)) ;
#15252 = CARTESIAN_POINT('',(73.6,44.2,34.5)) ;
#15253 = CARTESIAN_POINT('',(73.6,44.8,31.7193750595351)) ;
#15254 = CARTESIAN_POINT('',(73.6,44.8,34.5)) ;
#15255 = CARTESIAN_POINT('',(73.6,44.5,31.7193750595351)) ;
#15256 = CARTESIAN_POINT('Origin',(70.4,44.1,31.)) ;
#15257 = CARTESIAN_POINT('',(70.4,44.2,31.7193750595351)) ;
#15258 = CARTESIAN_POINT('',(70.4,44.2,33.)) ;
#15259 = CARTESIAN_POINT('',(70.4,44.8,31.7193750595351)) ;
#15260 = CARTESIAN_POINT('',(70.4,44.5,31.7193750595351)) ;
#15261 = CARTESIAN_POINT('',(70.4,44.8,33.)) ;
#15262 = CARTESIAN_POINT('Origin',(72.,44.5,35.)) ;
#15263 = CARTESIAN_POINT('Origin',(72.,44.8,35.)) ;
#15264 = CARTESIAN_POINT('Origin',(72.,44.2,35.)) ;
#15265 = CARTESIAN_POINT('Origin',(75.65,44.8,35.)) ;
#15266 = CARTESIAN_POINT('Origin',(72.,44.8,35.)) ;
#15267 = CARTESIAN_POINT('Origin',(72.,44.5,35.)) ;
#15268 = CARTESIAN_POINT('Origin',(72.,44.2,35.)) ;
#15269 = CARTESIAN_POINT('Origin',(73.6,44.2,35.)) ;
#15270 = CARTESIAN_POINT('',(0.,0.,0.)) ;
#15271 = CARTESIAN_POINT('Origin',(-68.9949895469777,49.9,44.4)) ;
#15272 = CARTESIAN_POINT('',(-76.3949895469778,49.9,44.4)) ;
#15273 = CARTESIAN_POINT('Origin',(-72.6949895469778,49.9,44.4)) ;
#15274 = CARTESIAN_POINT('Origin',(-72.6949895469778,49.75,44.4)) ;
#15275 = CARTESIAN_POINT('',(-76.6949895469778,49.6,44.4)) ;
#15276 = CARTESIAN_POINT('Origin',(-72.6949895469778,49.6,44.4)) ;
#15277 = CARTESIAN_POINT('',(-76.5449895469778,49.75,44.4)) ;
#15278 = CARTESIAN_POINT('Origin',(-72.6949895469778,48.9,44.4)) ;
#15279 = CARTESIAN_POINT('',(-76.6949895469778,48.2,44.4)) ;
#15280 = CARTESIAN_POINT('Origin',(-72.6949895469778,48.2,44.4)) ;
#15281 = CARTESIAN_POINT('',(-76.6949895469778,48.9,44.4)) ;
#15282 = CARTESIAN_POINT('Origin',(-72.6949895469778,48.05,44.4)) ;
#15283 = CARTESIAN_POINT('',(-76.3949895469778,47.9,44.4)) ;
#15284 = CARTESIAN_POINT('Origin',(-72.6949895469778,47.9,44.4)) ;
#15285 = CARTESIAN_POINT('',(-76.5449895469778,48.05,44.4)) ;
#15286 = CARTESIAN_POINT('Origin',(-71.1949895469778,47.9,44.4)) ;
#15287 = CARTESIAN_POINT('',(-74.1949895469778,47.9,44.4)) ;
#15288 = CARTESIAN_POINT('Origin',(-72.6949895469778,47.9,44.4)) ;
#15289 = CARTESIAN_POINT('Origin',(-72.6949895469778,46.45,44.4)) ;
#15290 = CARTESIAN_POINT('',(-74.1949895469778,45.,44.4)) ;
#15291 = CARTESIAN_POINT('Origin',(-72.6949895469778,45.,44.4)) ;
#15292 = CARTESIAN_POINT('',(-74.1949895469778,46.45,44.4)) ;
#15293 = CARTESIAN_POINT('Origin',(-72.6949895469778,44.9,44.4)) ;
#15294 = CARTESIAN_POINT('',(-73.9949895469777,44.8,44.4)) ;
#15295 = CARTESIAN_POINT('Origin',(-72.6949895469778,44.8,44.4)) ;
#15296 = CARTESIAN_POINT('',(-74.0949895469778,44.9,44.4)) ;
#15297 = CARTESIAN_POINT('Origin',(-72.6949895469778,44.8,44.4)) ;
#15298 = CARTESIAN_POINT('',(0.,0.,0.)) ;
#15299 = CARTESIAN_POINT('Origin',(84.75,52.3,26.4)) ;
#15300 = CARTESIAN_POINT('',(83.7822752358061,52.3006823179371,26.6289859168897)) ;
#15301 = CARTESIAN_POINT('',(83.7824753621529,52.3008465510102,26.5710140831103)) ;
#15302 = CARTESIAN_POINT('',(83.78325,52.3,26.4)) ;
#15303 = CARTESIAN_POINT('',(85.1756413254134,53.1688316687951,26.5)) ;
#15304 = CARTESIAN_POINT('Ctrl Pts',(83.7822752358061,52.3006823179371,26.6289859168897)) ;
#15305 = CARTESIAN_POINT('Ctrl Pts',(83.7819669536534,52.3408924644816,26.626330348121)) ;
#15306 = CARTESIAN_POINT('Ctrl Pts',(83.784257904817,52.381065877484,26.6236747793523)) ;
#15307 = CARTESIAN_POINT('Ctrl Pts',(83.7892671574507,52.4208955203977,26.6210192105835)) ;
#15308 = CARTESIAN_POINT('Ctrl Pts',(83.8289601627117,52.7365031252282,26.5999766493842)) ;
#15309 = CARTESIAN_POINT('Ctrl Pts',(84.0393320199538,53.0305258231898,26.5789340881849)) ;
#15310 = CARTESIAN_POINT('Ctrl Pts',(84.3252599776053,53.1701364250497,26.5578915269857)) ;
#15311 = CARTESIAN_POINT('Ctrl Pts',(84.5874715008695,53.2981669572095,26.5385943513238)) ;
#15312 = CARTESIAN_POINT('Ctrl Pts',(84.9132248715999,53.2963386188841,26.5192971756619)) ;
#15313 = CARTESIAN_POINT('Ctrl Pts',(85.1761635223117,53.1694011139097,26.5)) ;
#15314 = CARTESIAN_POINT('',(84.3248808714849,53.1682622236805,26.5)) ;
#15315 = CARTESIAN_POINT('Origin',(84.75,52.3,26.5)) ;
#15316 = CARTESIAN_POINT('Ctrl Pts',(84.3248808714849,53.1682622236805,26.5)) ;
#15317 = CARTESIAN_POINT('Ctrl Pts',(84.037889141541,53.0277451416316,26.5210425611993)) ;
#15318 = CARTESIAN_POINT('Ctrl Pts',(83.8284581828498,52.7349003276012,26.5420851223986)) ;
#15319 = CARTESIAN_POINT('Ctrl Pts',(83.7892954018501,52.419717415322,26.5631276835978)) ;
#15320 = CARTESIAN_POINT('Ctrl Pts',(83.7844028837125,52.3803423230635,26.5657564834353)) ;
#15321 = CARTESIAN_POINT('Ctrl Pts',(83.7821677312968,52.3406186013818,26.5683852832728)) ;
#15322 = CARTESIAN_POINT('Ctrl Pts',(83.7824753621529,52.3008465510102,26.5710140831103)) ;
#15323 = CARTESIAN_POINT('Origin',(84.75,52.3,26.4)) ;
#15324 = CARTESIAN_POINT('',(83.7847331702872,52.3001910598074,27.0289859168897)) ;
#15325 = CARTESIAN_POINT('',(83.7847326912755,52.3002006015805,26.9710140831103)) ;
#15326 = CARTESIAN_POINT('',(83.78325,52.3,26.4)) ;
#15327 = CARTESIAN_POINT('Ctrl Pts',(83.7847331702872,52.3001910598074,27.0289859168897)) ;
#15328 = CARTESIAN_POINT('Ctrl Pts',(83.7844687406298,52.4485469749339,27.0192523819834)) ;
#15329 = CARTESIAN_POINT('Ctrl Pts',(83.8166138594215,52.5967941566235,27.0095188470771)) ;
#15330 = CARTESIAN_POINT('Ctrl Pts',(83.881769803326,52.7287399208488,26.9997853121707)) ;
#15331 = CARTESIAN_POINT('Ctrl Pts',(84.0226279756452,53.013988481153,26.9787427509714)) ;
#15332 = CARTESIAN_POINT('Ctrl Pts',(84.3177671305919,53.2230499514336,26.9577001897721)) ;
#15333 = CARTESIAN_POINT('Ctrl Pts',(84.6335926430084,53.2612954524669,26.9366576285729)) ;
#15334 = CARTESIAN_POINT('Ctrl Pts',(84.9494181554248,53.2995409535003,26.9156150673736)) ;
#15335 = CARTESIAN_POINT('Ctrl Pts',(85.2859300253108,53.1669704852863,26.8945725061743)) ;
#15336 = CARTESIAN_POINT('Ctrl Pts',(85.4908016015415,52.9235850495878,26.873529944975)) ;
#15337 = CARTESIAN_POINT('Ctrl Pts',(85.6956731777722,52.6801996138893,26.8524873837757)) ;
#15338 = CARTESIAN_POINT('Ctrl Pts',(85.7689044603475,52.3259992107062,26.8314448225764)) ;
#15339 = CARTESIAN_POINT('Ctrl Pts',(85.677353054767,52.0213297802181,26.8104022613771)) ;
#15340 = CARTESIAN_POINT('Ctrl Pts',(85.5858016491865,51.7166603497299,26.7893597001778)) ;
#15341 = CARTESIAN_POINT('Ctrl Pts',(85.3294675554503,51.4615218919368,26.7683171389785)) ;
#15342 = CARTESIAN_POINT('Ctrl Pts',(85.0243692392349,51.371372572711,26.7472745777793)) ;
#15343 = CARTESIAN_POINT('Ctrl Pts',(84.7192709230194,51.2812232534852,26.72623201658)) ;
#15344 = CARTESIAN_POINT('Ctrl Pts',(84.3654083843247,51.3560630728268,26.7051894553807)) ;
#15345 = CARTESIAN_POINT('Ctrl Pts',(84.1229841916173,51.5620792383473,26.6841468941814)) ;
#15346 = CARTESIAN_POINT('Ctrl Pts',(83.9111539037505,51.7420961878111,26.6657599017508)) ;
#15347 = CARTESIAN_POINT('Ctrl Pts',(83.7844097621927,52.0222697726265,26.6473729093203)) ;
#15348 = CARTESIAN_POINT('Ctrl Pts',(83.7822752358061,52.3006823179371,26.6289859168897)) ;
#15349 = CARTESIAN_POINT('Ctrl Pts',(83.7824753621529,52.3008465510102,26.5710140831103)) ;
#15350 = CARTESIAN_POINT('Ctrl Pts',(83.7846302014414,52.0222581876176,26.5894278444721)) ;
#15351 = CARTESIAN_POINT('Ctrl Pts',(83.9115461789277,51.7412985869987,26.6078416058339)) ;
#15352 = CARTESIAN_POINT('Ctrl Pts',(84.1238435334506,51.5611752748842,26.6262553671957)) ;
#15353 = CARTESIAN_POINT('Ctrl Pts',(84.366449049359,51.3553370572536,26.647297928395)) ;
#15354 = CARTESIAN_POINT('Ctrl Pts',(84.720554684484,51.2811816325205,26.6683404895943)) ;
#15355 = CARTESIAN_POINT('Ctrl Pts',(85.0255768160984,51.3717764490523,26.6893830507936)) ;
#15356 = CARTESIAN_POINT('Ctrl Pts',(85.3305989477127,51.4623712655841,26.7104256119929)) ;
#15357 = CARTESIAN_POINT('Ctrl Pts',(85.5865375758163,51.7177163233807,26.7314681731922)) ;
#15358 = CARTESIAN_POINT('Ctrl Pts',(85.6776859602006,52.0224714271219,26.7525107343915)) ;
#15359 = CARTESIAN_POINT('Ctrl Pts',(85.7688343445849,52.3272265308631,26.7735532955908)) ;
#15360 = CARTESIAN_POINT('Ctrl Pts',(85.6951924852498,52.6813916805489,26.79459585679)) ;
#15361 = CARTESIAN_POINT('Ctrl Pts',(85.4900232232115,52.9245330496733,26.8156384179893)) ;
#15362 = CARTESIAN_POINT('Ctrl Pts',(85.2848539611732,53.1676744187977,26.8366809791886)) ;
#15363 = CARTESIAN_POINT('Ctrl Pts',(84.9481572964317,53.2997920073608,26.8577235403879)) ;
#15364 = CARTESIAN_POINT('Ctrl Pts',(84.6323757540708,53.2611409632297,26.8787661015872)) ;
#15365 = CARTESIAN_POINT('Ctrl Pts',(84.3165942117099,53.2224899190985,26.8998086627865)) ;
#15366 = CARTESIAN_POINT('Ctrl Pts',(84.0217277917296,53.0130702422731,26.9208512239858)) ;
#15367 = CARTESIAN_POINT('Ctrl Pts',(83.8812317852022,52.7276477521024,26.9418937851851)) ;
#15368 = CARTESIAN_POINT('Ctrl Pts',(83.8164220957884,52.5959846294495,26.9516005511601)) ;
#15369 = CARTESIAN_POINT('Ctrl Pts',(83.7844609400415,52.4481488418597,26.9613073171352)) ;
#15370 = CARTESIAN_POINT('Ctrl Pts',(83.7847326912755,52.3002006015805,26.9710140831103)) ;
#15371 = CARTESIAN_POINT('Origin',(84.75,52.3,26.4)) ;
#15372 = CARTESIAN_POINT('',(83.7829231651454,52.2991702952661,27.4289859168897)) ;
#15373 = CARTESIAN_POINT('',(83.7829351910593,52.2991686072217,27.3710140831103)) ;
#15374 = CARTESIAN_POINT('',(83.78325,52.3,26.4)) ;
#15375 = CARTESIAN_POINT('Ctrl Pts',(83.7829231651454,52.2991702952661,27.4289859168897)) ;
#15376 = CARTESIAN_POINT('Ctrl Pts',(83.7852242648531,52.5541918641273,27.4121744158458)) ;
#15377 = CARTESIAN_POINT('Ctrl Pts',(83.8890401093448,52.810871192434,27.3953629148018)) ;
#15378 = CARTESIAN_POINT('Ctrl Pts',(84.0699842686843,52.9893621083363,27.3785514137579)) ;
#15379 = CARTESIAN_POINT('Ctrl Pts',(84.2964678251858,53.2127749976184,27.3575088525586)) ;
#15380 = CARTESIAN_POINT('Ctrl Pts',(84.6437878592095,53.3136905607676,27.3364662913593)) ;
#15381 = CARTESIAN_POINT('Ctrl Pts',(84.9547283733474,53.2464289555923,27.3154237301601)) ;
#15382 = CARTESIAN_POINT('Ctrl Pts',(85.2656688874853,53.1791673504169,27.2943811689608)) ;
#15383 = CARTESIAN_POINT('Ctrl Pts',(85.5402298817374,52.9437285769171,27.2733386077615)) ;
#15384 = CARTESIAN_POINT('Ctrl Pts',(85.6541300102328,52.6466849747208,27.2522960465622)) ;
#15385 = CARTESIAN_POINT('Ctrl Pts',(85.7680301387282,52.3496413725244,27.2312534853629)) ;
#15386 = CARTESIAN_POINT('Ctrl Pts',(85.7212694014668,51.9909929416316,27.2102109241636)) ;
#15387 = CARTESIAN_POINT('Ctrl Pts',(85.5350143493848,51.7330837735866,27.1891683629643)) ;
#15388 = CARTESIAN_POINT('Ctrl Pts',(85.3487592973027,51.4751746055417,27.168125801765)) ;
#15389 = CARTESIAN_POINT('Ctrl Pts',(85.0230099303999,51.3180047003446,27.1470832405657)) ;
#15390 = CARTESIAN_POINT('Ctrl Pts',(84.7052180283029,51.3327172918697,27.1260406793665)) ;
#15391 = CARTESIAN_POINT('Ctrl Pts',(84.387426126206,51.3474298833948,27.1049981181672)) ;
#15392 = CARTESIAN_POINT('Ctrl Pts',(84.0775916889149,51.534024971642,27.0839555569679)) ;
#15393 = CARTESIAN_POINT('Ctrl Pts',(83.9159630651151,51.8080403409294,27.0629129957686)) ;
#15394 = CARTESIAN_POINT('Ctrl Pts',(83.8290980519193,51.9553060176977,27.0516039694756)) ;
#15395 = CARTESIAN_POINT('Ctrl Pts',(83.785040401111,52.1278219296783,27.0402949431826)) ;
#15396 = CARTESIAN_POINT('Ctrl Pts',(83.7847331702872,52.3001910598074,27.0289859168897)) ;
#15397 = CARTESIAN_POINT('Ctrl Pts',(83.7847326912755,52.3002006015805,26.9710140831103)) ;
#15398 = CARTESIAN_POINT('Ctrl Pts',(83.7850500489154,52.1274230812518,26.9823498783345)) ;
#15399 = CARTESIAN_POINT('Ctrl Pts',(83.8293270681539,51.9544921964693,26.9936856735587)) ;
#15400 = CARTESIAN_POINT('Ctrl Pts',(83.9165832441649,51.8069869482407,27.0050214687829)) ;
#15401 = CARTESIAN_POINT('Ctrl Pts',(84.0785563027296,51.5331739380657,27.0260640299822)) ;
#15402 = CARTESIAN_POINT('Ctrl Pts',(84.3886280129336,51.3469732212317,27.0471065911815)) ;
#15403 = CARTESIAN_POINT('Ctrl Pts',(84.7064387677917,51.3326623797936,27.0681491523808)) ;
#15404 = CARTESIAN_POINT('Ctrl Pts',(85.0242495226499,51.3183515383555,27.0891917135801)) ;
#15405 = CARTESIAN_POINT('Ctrl Pts',(85.3497993221623,51.4759305723135,27.1102342747794)) ;
#15406 = CARTESIAN_POINT('Ctrl Pts',(85.5357286216791,51.7340740692188,27.1312768359787)) ;
#15407 = CARTESIAN_POINT('Ctrl Pts',(85.7216579211959,51.9922175661241,27.152319397178)) ;
#15408 = CARTESIAN_POINT('Ctrl Pts',(85.7679667207172,52.3509255259768,27.1733619583772)) ;
#15409 = CARTESIAN_POINT('Ctrl Pts',(85.6536921048407,52.6478254252983,27.1944045195765)) ;
#15410 = CARTESIAN_POINT('Ctrl Pts',(85.5394174889643,52.9447253246197,27.2154470807758)) ;
#15411 = CARTESIAN_POINT('Ctrl Pts',(85.2645594576901,53.1798171634098,27.2364896419751)) ;
#15412 = CARTESIAN_POINT('Ctrl Pts',(84.9535342733738,53.2466863758117,27.2575322031744)) ;
#15413 = CARTESIAN_POINT('Ctrl Pts',(84.6425090890574,53.3135555882136,27.2785747643737)) ;
#15414 = CARTESIAN_POINT('Ctrl Pts',(84.2953167516988,53.2122021742272,27.299617325573)) ;
#15415 = CARTESIAN_POINT('Ctrl Pts',(84.0691152289107,52.9885038104687,27.3206598867723)) ;
#15416 = CARTESIAN_POINT('Ctrl Pts',(83.8886841526971,52.8100693948966,27.3374446188849)) ;
#15417 = CARTESIAN_POINT('Ctrl Pts',(83.7852341620669,52.5537923176105,27.3542293509976)) ;
#15418 = CARTESIAN_POINT('Ctrl Pts',(83.7829351910593,52.2991686072217,27.3710140831103)) ;
#15419 = CARTESIAN_POINT('Origin',(84.75,52.3,26.4)) ;
#15420 = CARTESIAN_POINT('',(83.782331408344,52.3006703987026,27.8289859168897)) ;
#15421 = CARTESIAN_POINT('',(83.7823209222831,52.3006659823901,27.7710140831103)) ;
#15422 = CARTESIAN_POINT('',(83.78325,52.3,26.4)) ;
#15423 = CARTESIAN_POINT('Ctrl Pts',(83.782331408344,52.3006703987026,27.8289859168897)) ;
#15424 = CARTESIAN_POINT('Ctrl Pts',(83.7819893417447,52.3437879615906,27.8261390109074)) ;
#15425 = CARTESIAN_POINT('Ctrl Pts',(83.7846250624964,52.3868634658397,27.8232921049252)) ;
#15426 = CARTESIAN_POINT('Ctrl Pts',(83.7903820188789,52.4295177032146,27.820445198943)) ;
#15427 = CARTESIAN_POINT('Ctrl Pts',(83.8329338656059,52.744791339215,27.7994026377437)) ;
#15428 = CARTESIAN_POINT('Ctrl Pts',(84.0460065682424,53.0370501194155,27.7783600765444)) ;
#15429 = CARTESIAN_POINT('Ctrl Pts',(84.3331517830637,53.1740017558885,27.7573175153451)) ;
#15430 = CARTESIAN_POINT('Ctrl Pts',(84.6202969978849,53.3109533923615,27.7362749541458)) ;
#15431 = CARTESIAN_POINT('Ctrl Pts',(84.9815147248909,53.2925978851069,27.7152323929466)) ;
#15432 = CARTESIAN_POINT('Ctrl Pts',(85.2532980908674,53.1272439400855,27.6941898317473)) ;
#15433 = CARTESIAN_POINT('Ctrl Pts',(85.5250814568439,52.9618899950641,27.673147270548)) ;
#15434 = CARTESIAN_POINT('Ctrl Pts',(85.7074304617909,52.6495376122759,27.6521047093487)) ;
#15435 = CARTESIAN_POINT('Ctrl Pts',(85.7178039852687,52.3315745397791,27.6310621481494)) ;
#15436 = CARTESIAN_POINT('Ctrl Pts',(85.7281775087464,52.0136114672823,27.6100195869501)) ;
#15437 = CARTESIAN_POINT('Ctrl Pts',(85.5665755507549,51.6900377050768,27.5889770257508)) ;
#15438 = CARTESIAN_POINT('Ctrl Pts',(85.3061479856785,51.5073204152145,27.5679344645515)) ;
#15439 = CARTESIAN_POINT('Ctrl Pts',(85.0457204206021,51.3246031253523,27.5468919033522)) ;
#15440 = CARTESIAN_POINT('Ctrl Pts',(84.6864672484407,51.2827423078331,27.5258493421529)) ;
#15441 = CARTESIAN_POINT('Ctrl Pts',(84.3910060753508,51.4006864487252,27.5048067809536)) ;
#15442 = CARTESIAN_POINT('Ctrl Pts',(84.095544902261,51.5186305896173,27.4837642197543)) ;
#15443 = CARTESIAN_POINT('Ctrl Pts',(83.8638757282426,51.7963796889206,27.4627216585551)) ;
#15444 = CARTESIAN_POINT('Ctrl Pts',(83.8008646807231,52.1082093462798,27.4416790973558)) ;
#15445 = CARTESIAN_POINT('Ctrl Pts',(83.7881949524527,52.1709094152505,27.4374480372004)) ;
#15446 = CARTESIAN_POINT('Ctrl Pts',(83.7823440323683,52.2349873531273,27.4332169770451)) ;
#15447 = CARTESIAN_POINT('Ctrl Pts',(83.7829231651454,52.2991702952661,27.4289859168897)) ;
#15448 = CARTESIAN_POINT('Ctrl Pts',(83.7829351910593,52.2991686072217,27.3710140831103)) ;
#15449 = CARTESIAN_POINT('Ctrl Pts',(83.7823520047707,52.2345775114,27.3752719121969)) ;
#15450 = CARTESIAN_POINT('Ctrl Pts',(83.7882778726445,52.1700928095101,27.3795297412835)) ;
#15451 = CARTESIAN_POINT('Ctrl Pts',(83.8011073400004,52.1070121793185,27.3837875703701)) ;
#15452 = CARTESIAN_POINT('Ctrl Pts',(83.8645116820959,51.7952622254577,27.4048301315694)) ;
#15453 = CARTESIAN_POINT('Ctrl Pts',(84.0965310745045,51.5178056312668,27.4258726927687)) ;
#15454 = CARTESIAN_POINT('Ctrl Pts',(84.3921408066335,51.4002343057104,27.446915253968)) ;
#15455 = CARTESIAN_POINT('Ctrl Pts',(84.6877505387624,51.2826629801539,27.4679578151673)) ;
#15456 = CARTESIAN_POINT('Ctrl Pts',(85.0469506106117,51.3249769232318,27.4890003763666)) ;
#15457 = CARTESIAN_POINT('Ctrl Pts',(85.307147479323,51.5080225826629,27.5100429375659)) ;
#15458 = CARTESIAN_POINT('Ctrl Pts',(85.5673443480344,51.691068242094,27.5310854987651)) ;
#15459 = CARTESIAN_POINT('Ctrl Pts',(85.7285380136077,52.0148456178783,27.5521280599644)) ;
#15460 = CARTESIAN_POINT('Ctrl Pts',(85.7177634037076,52.3327953600667,27.5731706211637)) ;
#15461 = CARTESIAN_POINT('Ctrl Pts',(85.7069887938075,52.6507451022551,27.594213182363)) ;
#15462 = CARTESIAN_POINT('Ctrl Pts',(85.5242459084338,52.9628672108476,27.6152557435623)) ;
#15463 = CARTESIAN_POINT('Ctrl Pts',(85.2522541664254,53.1278781829457,27.6362983047616)) ;
#15464 = CARTESIAN_POINT('Ctrl Pts',(84.9802624244171,53.2928891550439,27.6573408659609)) ;
#15465 = CARTESIAN_POINT('Ctrl Pts',(84.6190218257741,53.3107889906478,27.6783834271602)) ;
#15466 = CARTESIAN_POINT('Ctrl Pts',(84.3320495934087,53.1734752405106,27.6994259883595)) ;
#15467 = CARTESIAN_POINT('Ctrl Pts',(84.0450773610434,53.0361614903734,27.7204685495587)) ;
#15468 = CARTESIAN_POINT('Ctrl Pts',(83.8323734949557,52.7436341544952,27.741511110758)) ;
#15469 = CARTESIAN_POINT('Ctrl Pts',(83.7902193849058,52.4283070863173,27.7625536719573)) ;
#15470 = CARTESIAN_POINT('Ctrl Pts',(83.7845698650361,52.3860467578464,27.7653738090083)) ;
#15471 = CARTESIAN_POINT('Ctrl Pts',(83.7819836790408,52.3433769113913,27.7681939460593)) ;
#15472 = CARTESIAN_POINT('Ctrl Pts',(83.7823209222831,52.3006659823901,27.7710140831103)) ;
#15473 = CARTESIAN_POINT('Origin',(84.75,52.3,26.4)) ;
#15474 = CARTESIAN_POINT('',(83.7847482189314,52.300144797748,28.2289859168897)) ;
#15475 = CARTESIAN_POINT('',(83.784746322328,52.3001512320295,28.1710140831103)) ;
#15476 = CARTESIAN_POINT('',(83.78325,52.3,26.4)) ;
#15477 = CARTESIAN_POINT('Ctrl Pts',(83.7847482189314,52.300144797748,28.2289859168897)) ;
#15478 = CARTESIAN_POINT('Ctrl Pts',(83.7845434991546,52.451422798205,28.2190610447698)) ;
#15479 = CARTESIAN_POINT('Ctrl Pts',(83.8180233821541,52.6026150775528,28.20913617265)) ;
#15480 = CARTESIAN_POINT('Ctrl Pts',(83.8856705962109,52.7365503256865,28.1992113005302)) ;
#15481 = CARTESIAN_POINT('Ctrl Pts',(84.0290951788721,53.0205177785228,28.1781687393309)) ;
#15482 = CARTESIAN_POINT('Ctrl Pts',(84.3261081608466,53.2269117212532,28.1571261781316)) ;
#15483 = CARTESIAN_POINT('Ctrl Pts',(84.6422652431795,53.2623069818343,28.1360836169323)) ;
#15484 = CARTESIAN_POINT('Ctrl Pts',(84.9584223255125,53.2977022424154,28.115041055733)) ;
#15485 = CARTESIAN_POINT('Ctrl Pts',(85.2937235082039,53.1620988208472,28.0939984945337)) ;
#15486 = CARTESIAN_POINT('Ctrl Pts',(85.4963931612999,52.9168782326122,28.0729559333344)) ;
#15487 = CARTESIAN_POINT('Ctrl Pts',(85.6990628143959,52.6716576443773,28.0519133721352)) ;
#15488 = CARTESIAN_POINT('Ctrl Pts',(85.7691009378964,52.3168198894756,28.0308708109359)) ;
#15489 = CARTESIAN_POINT('Ctrl Pts',(85.6748044515052,52.0129839175434,28.0098282497366)) ;
#15490 = CARTESIAN_POINT('Ctrl Pts',(85.5805079651139,51.7091479456112,27.9887856885373)) ;
#15491 = CARTESIAN_POINT('Ctrl Pts',(85.3218768688308,51.4563137566485,27.967743127338)) ;
#15492 = CARTESIAN_POINT('Ctrl Pts',(85.0159817236842,51.3689279148218,27.9467005661387)) ;
#15493 = CARTESIAN_POINT('Ctrl Pts',(84.7100865785376,51.2815420729951,27.9256580049394)) ;
#15494 = CARTESIAN_POINT('Ctrl Pts',(84.3569273845274,51.3596045783045,27.9046154437401)) ;
#15495 = CARTESIAN_POINT('Ctrl Pts',(84.116363282931,51.5677800768593,27.8835728825408)) ;
#15496 = CARTESIAN_POINT('Ctrl Pts',(83.9083457603114,51.7477909396278,27.8653772273238)) ;
#15497 = CARTESIAN_POINT('Ctrl Pts',(83.7845176856361,52.0250897111043,27.8471815721067)) ;
#15498 = CARTESIAN_POINT('Ctrl Pts',(83.782331408344,52.3006703987026,27.8289859168897)) ;
#15499 = CARTESIAN_POINT('Ctrl Pts',(83.7823209222831,52.3006659823901,27.7710140831103)) ;
#15500 = CARTESIAN_POINT('Ctrl Pts',(83.7845000324795,52.0246876700055,27.7892365072586)) ;
#15501 = CARTESIAN_POINT('Ctrl Pts',(83.9087366396395,51.7469941005196,27.8074589314069)) ;
#15502 = CARTESIAN_POINT('Ctrl Pts',(84.1172874394612,51.5669813423512,27.8256813555552)) ;
#15503 = CARTESIAN_POINT('Ctrl Pts',(84.3581139580789,51.3591094670406,27.8467239167545)) ;
#15504 = CARTESIAN_POINT('Ctrl Pts',(84.7113713493266,51.281492516897,27.8677664779538)) ;
#15505 = CARTESIAN_POINT('Ctrl Pts',(85.0171560228832,51.369264163824,27.8888090391531)) ;
#15506 = CARTESIAN_POINT('Ctrl Pts',(85.3229406964397,51.4570358107511,27.9098516003523)) ;
#15507 = CARTESIAN_POINT('Ctrl Pts',(85.5812526523051,51.7101960547489,27.9308941615516)) ;
#15508 = CARTESIAN_POINT('Ctrl Pts',(85.675165789644,52.0141507410278,27.9519367227509)) ;
#15509 = CARTESIAN_POINT('Ctrl Pts',(85.769078926983,52.3181054273066,27.9729792839502)) ;
#15510 = CARTESIAN_POINT('Ctrl Pts',(85.6985932457955,52.6728545558666,27.9940218451495)) ;
#15511 = CARTESIAN_POINT('Ctrl Pts',(85.495614415528,52.9178192943447,28.0150644063488)) ;
#15512 = CARTESIAN_POINT('Ctrl Pts',(85.2926355852604,53.1627840328228,28.0361069675481)) ;
#15513 = CARTESIAN_POINT('Ctrl Pts',(84.9571636059129,53.297964381219,28.0571495287474)) ;
#15514 = CARTESIAN_POINT('Ctrl Pts',(84.6410514192883,53.2621703300033,28.0781920899466)) ;
#15515 = CARTESIAN_POINT('Ctrl Pts',(84.3249392326637,53.2263762787877,28.0992346511459)) ;
#15516 = CARTESIAN_POINT('Ctrl Pts',(84.0281868387621,53.0196078279602,28.1202772123452)) ;
#15517 = CARTESIAN_POINT('Ctrl Pts',(83.8851205801658,52.7354596724217,28.1413197735445)) ;
#15518 = CARTESIAN_POINT('Ctrl Pts',(83.8178243714495,52.6018006687607,28.1512178767331)) ;
#15519 = CARTESIAN_POINT('Ctrl Pts',(83.7845330583397,52.4510204799289,28.1611159799217)) ;
#15520 = CARTESIAN_POINT('Ctrl Pts',(83.784746322328,52.3001512320295,28.1710140831103)) ;
#15521 = CARTESIAN_POINT('Origin',(84.75,52.3,26.4)) ;
#15522 = CARTESIAN_POINT('',(83.7828374094831,52.29918392718,28.6289859168897)) ;
#15523 = CARTESIAN_POINT('',(83.7828493504888,52.2991818538181,28.5710140831103)) ;
#15524 = CARTESIAN_POINT('',(83.78325,52.3,26.4)) ;
#15525 = CARTESIAN_POINT('Ctrl Pts',(83.7828374094831,52.29918392718,28.6289859168897)) ;
#15526 = CARTESIAN_POINT('Ctrl Pts',(83.7851495737918,52.5570489842384,28.6119830786322)) ;
#15527 = CARTESIAN_POINT('Ctrl Pts',(83.8916037184267,52.8166003859073,28.5949802403748)) ;
#15528 = CARTESIAN_POINT('Ctrl Pts',(84.0762274939135,52.9954653946484,28.5779774021174)) ;
#15529 = CARTESIAN_POINT('Ctrl Pts',(84.3047162341877,53.2168271364859,28.5569348409181)) ;
#15530 = CARTESIAN_POINT('Ctrl Pts',(84.6529320602892,53.3146070398796,28.5358922797188)) ;
#15531 = CARTESIAN_POINT('Ctrl Pts',(84.9632534692345,53.2445445796632,28.5148497185195)) ;
#15532 = CARTESIAN_POINT('Ctrl Pts',(85.2735748781798,53.1744821194467,28.4938071573202)) ;
#15533 = CARTESIAN_POINT('Ctrl Pts',(85.5460018699689,52.93657729562,28.4727645961209)) ;
#15534 = CARTESIAN_POINT('Ctrl Pts',(85.6572191077321,52.6385188261787,28.4517220349216)) ;
#15535 = CARTESIAN_POINT('Ctrl Pts',(85.7684363454952,52.3404603567374,28.4306794737223)) ;
#15536 = CARTESIAN_POINT('Ctrl Pts',(85.7184438292325,51.9822482416814,28.4096369125231)) ;
#15537 = CARTESIAN_POINT('Ctrl Pts',(85.5298709024732,51.7260288503878,28.3885943513238)) ;
#15538 = CARTESIAN_POINT('Ctrl Pts',(85.3412979757139,51.4698094590941,28.3675517901245)) ;
#15539 = CARTESIAN_POINT('Ctrl Pts',(85.0141446384581,51.3155827915627,28.3465092289252)) ;
#15540 = CARTESIAN_POINT('Ctrl Pts',(84.6964983607722,51.3331602616194,28.3254666677259)) ;
#15541 = CARTESIAN_POINT('Ctrl Pts',(84.3788520830862,51.3507377316761,28.3044241065266)) ;
#15542 = CARTESIAN_POINT('Ctrl Pts',(84.07071286497,51.5401193393208,28.2833815453273)) ;
#15543 = CARTESIAN_POINT('Ctrl Pts',(83.9115613475859,51.8155806246143,28.262338984128)) ;
#15544 = CARTESIAN_POINT('Ctrl Pts',(83.8274747637313,51.9611186555753,28.2512212950486)) ;
#15545 = CARTESIAN_POINT('Ctrl Pts',(83.7849775428762,52.1306855086675,28.2401036059691)) ;
#15546 = CARTESIAN_POINT('Ctrl Pts',(83.7847482189314,52.300144797748,28.2289859168897)) ;
#15547 = CARTESIAN_POINT('Ctrl Pts',(83.784746322328,52.3001512320295,28.1710140831103)) ;
#15548 = CARTESIAN_POINT('Ctrl Pts',(83.784986440209,52.1302847468775,28.182158541121)) ;
#15549 = CARTESIAN_POINT('Ctrl Pts',(83.8277000620734,51.9603053622059,28.1933029991317)) ;
#15550 = CARTESIAN_POINT('Ctrl Pts',(83.9121730740077,51.8145233484151,28.2044474571424)) ;
#15551 = CARTESIAN_POINT('Ctrl Pts',(84.0716719497369,51.5392630401967,28.2254900183417)) ;
#15552 = CARTESIAN_POINT('Ctrl Pts',(84.3800498244863,51.3502702840097,28.246532579541)) ;
#15553 = CARTESIAN_POINT('Ctrl Pts',(84.6977180280713,51.3330935243927,28.2675751407402)) ;
#15554 = CARTESIAN_POINT('Ctrl Pts',(85.0153862316564,51.3159167647757,28.2886177019395)) ;
#15555 = CARTESIAN_POINT('Ctrl Pts',(85.342344764077,51.4705560017287,28.3096602631388)) ;
#15556 = CARTESIAN_POINT('Ctrl Pts',(85.530594334573,51.7270130699661,28.3307028243381)) ;
#15557 = CARTESIAN_POINT('Ctrl Pts',(85.7188439050691,51.9834701382036,28.3517453855374)) ;
#15558 = CARTESIAN_POINT('Ctrl Pts',(85.7683845136405,52.3417450377255,28.3727879467367)) ;
#15559 = CARTESIAN_POINT('Ctrl Pts',(85.6567913748644,52.6396629794784,28.393830507936)) ;
#15560 = CARTESIAN_POINT('Ctrl Pts',(85.5451982360883,52.9375809212313,28.4148730691353)) ;
#15561 = CARTESIAN_POINT('Ctrl Pts',(85.2724713499645,53.1751419052153,28.4359156303346)) ;
#15562 = CARTESIAN_POINT('Ctrl Pts',(84.9620618019187,53.2448128541275,28.4569581915338)) ;
#15563 = CARTESIAN_POINT('Ctrl Pts',(84.6516522538729,53.3144838030397,28.4780007527331)) ;
#15564 = CARTESIAN_POINT('Ctrl Pts',(84.3035600439051,53.2162647168803,28.4990433139324)) ;
#15565 = CARTESIAN_POINT('Ctrl Pts',(84.0753507195849,52.9946149189247,28.5200858751317)) ;
#15566 = CARTESIAN_POINT('Ctrl Pts',(83.8912430307036,52.8157991226631,28.5370619444579)) ;
#15567 = CARTESIAN_POINT('Ctrl Pts',(83.7851604304188,52.5566491555032,28.5540380137841)) ;
#15568 = CARTESIAN_POINT('Ctrl Pts',(83.7828493504888,52.2991818538181,28.5710140831103)) ;
#15569 = CARTESIAN_POINT('Origin',(84.75,52.3,26.4)) ;
#15570 = CARTESIAN_POINT('',(83.782407671779,52.3007005599052,29.0289859168897)) ;
#15571 = CARTESIAN_POINT('',(83.782396840654,52.3006964898307,28.9710140831103)) ;
#15572 = CARTESIAN_POINT('',(83.78325,52.3,26.4)) ;
#15573 = CARTESIAN_POINT('Ctrl Pts',(83.782407671779,52.3007005599052,29.0289859168897)) ;
#15574 = CARTESIAN_POINT('Ctrl Pts',(83.7820311033026,52.3467254751765,29.0259476736939)) ;
#15575 = CARTESIAN_POINT('Ctrl Pts',(83.7850347520562,52.3927010359488,29.0229094304982)) ;
#15576 = CARTESIAN_POINT('Ctrl Pts',(83.7915888137738,52.4381647684036,29.0198711873024)) ;
#15577 = CARTESIAN_POINT('Ctrl Pts',(83.8369815739682,52.7530419230263,28.9988286261032)) ;
#15578 = CARTESIAN_POINT('Ctrl Pts',(84.0526807466604,53.0433676675877,28.9777860649039)) ;
#15579 = CARTESIAN_POINT('Ctrl Pts',(84.3410491044655,53.1777247120556,28.9567435037046)) ;
#15580 = CARTESIAN_POINT('Ctrl Pts',(84.6294174622707,53.3120817565235,28.9357009425053)) ;
#15581 = CARTESIAN_POINT('Ctrl Pts',(84.9904550051888,53.2904701008978,28.914658381306)) ;
#15582 = CARTESIAN_POINT('Ctrl Pts',(85.2607364208631,53.122672360977,28.8936158201067)) ;
#15583 = CARTESIAN_POINT('Ctrl Pts',(85.5310178365373,52.9548746210563,28.8725732589074)) ;
#15584 = CARTESIAN_POINT('Ctrl Pts',(85.7105431249676,52.6408907968403,28.8515306977081)) ;
#15585 = CARTESIAN_POINT('Ctrl Pts',(85.71804933466,52.3228471174543,28.8304881365088)) ;
#15586 = CARTESIAN_POINT('Ctrl Pts',(85.7255555443523,52.0048034380682,28.8094455753095)) ;
#15587 = CARTESIAN_POINT('Ctrl Pts',(85.5610426753067,51.6826999035119,28.7884030141103)) ;
#15588 = CARTESIAN_POINT('Ctrl Pts',(85.2989782380021,51.5023381673217,28.767360452911)) ;
#15589 = CARTESIAN_POINT('Ctrl Pts',(85.0369138006973,51.3219764311315,28.7463178917117)) ;
#15590 = CARTESIAN_POINT('Ctrl Pts',(84.6772977951335,51.2833564933073,28.7252753305124)) ;
#15591 = CARTESIAN_POINT('Ctrl Pts',(84.3829120682143,51.4039598471894,28.7042327693131)) ;
#15592 = CARTESIAN_POINT('Ctrl Pts',(84.0885263412951,51.5245632010715,28.6831902081138)) ;
#15593 = CARTESIAN_POINT('Ctrl Pts',(83.8593708930204,51.80438984666,28.6621476469145)) ;
#15594 = CARTESIAN_POINT('Ctrl Pts',(83.7991739961065,52.1167749595949,28.6411050857152)) ;
#15595 = CARTESIAN_POINT('Ctrl Pts',(83.7876174758146,52.1767462385407,28.6370653627734)) ;
#15596 = CARTESIAN_POINT('Ctrl Pts',(83.7822880598356,52.2379174861818,28.6330256398315)) ;
#15597 = CARTESIAN_POINT('Ctrl Pts',(83.7828374094831,52.29918392718,28.6289859168897)) ;
#15598 = CARTESIAN_POINT('Ctrl Pts',(83.7828493504888,52.2991818538181,28.5710140831103)) ;
#15599 = CARTESIAN_POINT('Ctrl Pts',(83.7822957483815,52.237507465609,28.5750805749834)) ;
#15600 = CARTESIAN_POINT('Ctrl Pts',(83.7876966245727,52.175929629855,28.5791470668565)) ;
#15601 = CARTESIAN_POINT('Ctrl Pts',(83.799405866669,52.115575677217,28.5832135587296)) ;
#15602 = CARTESIAN_POINT('Ctrl Pts',(83.8599967767458,51.8032667432166,28.6042561199289)) ;
#15603 = CARTESIAN_POINT('Ctrl Pts',(84.0895050355717,51.5237293849677,28.6252986811282)) ;
#15604 = CARTESIAN_POINT('Ctrl Pts',(84.3840426691043,51.4034974795791,28.6463412423274)) ;
#15605 = CARTESIAN_POINT('Ctrl Pts',(84.678580302637,51.2832655741904,28.6673838035267)) ;
#15606 = CARTESIAN_POINT('Ctrl Pts',(85.0381473108762,51.3223391216621,28.688426364726)) ;
#15607 = CARTESIAN_POINT('Ctrl Pts',(85.2999840257837,51.5030313001503,28.7094689259253)) ;
#15608 = CARTESIAN_POINT('Ctrl Pts',(85.5618207406912,51.6837234786386,28.7305114871246)) ;
#15609 = CARTESIAN_POINT('Ctrl Pts',(85.7259271622669,52.0060342881435,28.7515540483239)) ;
#15610 = CARTESIAN_POINT('Ctrl Pts',(85.7180197603577,52.3240682511654,28.7725966095232)) ;
#15611 = CARTESIAN_POINT('Ctrl Pts',(85.7101123584486,52.6421022141873,28.7936391707225)) ;
#15612 = CARTESIAN_POINT('Ctrl Pts',(85.5301911330546,52.9558593307262,28.8146817319218)) ;
#15613 = CARTESIAN_POINT('Ctrl Pts',(85.2596982583662,53.1233159919349,28.835724293121)) ;
#15614 = CARTESIAN_POINT('Ctrl Pts',(84.9892053836778,53.2907726531436,28.8567668543203)) ;
#15615 = CARTESIAN_POINT('Ctrl Pts',(84.628140859695,53.3119288590221,28.8778094155196)) ;
#15616 = CARTESIAN_POINT('Ctrl Pts',(84.3399422118783,53.1772081552049,28.8988519767189)) ;
#15617 = CARTESIAN_POINT('Ctrl Pts',(84.0517435640616,53.0424874513877,28.9198945379182)) ;
#15618 = CARTESIAN_POINT('Ctrl Pts',(83.836410792411,52.7518898378748,28.9409370991175)) ;
#15619 = CARTESIAN_POINT('Ctrl Pts',(83.7914152711865,52.4369556674358,28.9619796603168)) ;
#15620 = CARTESIAN_POINT('Ctrl Pts',(83.784975805339,52.3918843407893,28.9649911345813)) ;
#15621 = CARTESIAN_POINT('Ctrl Pts',(83.7820250967013,52.3463145656929,28.9680026088458)) ;
#15622 = CARTESIAN_POINT('Ctrl Pts',(83.782396840654,52.3006964898307,28.9710140831103)) ;
#15623 = CARTESIAN_POINT('Origin',(84.75,52.3,26.4)) ;
#15624 = CARTESIAN_POINT('',(83.7847592665387,52.3000985915647,29.4289859168897)) ;
#15625 = CARTESIAN_POINT('',(83.784757957323,52.3001050761132,29.3710140831103)) ;
#15626 = CARTESIAN_POINT('',(83.78325,52.3,26.4)) ;
#15627 = CARTESIAN_POINT('Ctrl Pts',(83.7847592665387,52.3000985915647,29.4289859168897)) ;
#15628 = CARTESIAN_POINT('Ctrl Pts',(83.7846172807008,52.4542974257026,29.4188697075563)) ;
#15629 = CARTESIAN_POINT('Ctrl Pts',(83.8194624052769,52.6084356653519,29.408753498223)) ;
#15630 = CARTESIAN_POINT('Ctrl Pts',(83.8896418563525,52.7443257473643,29.3986372888896)) ;
#15631 = CARTESIAN_POINT('Ctrl Pts',(84.035620982083,53.0269884793123,29.3775947276903)) ;
#15632 = CARTESIAN_POINT('Ctrl Pts',(84.3344828276875,53.2306960351298,29.3565521664911)) ;
#15633 = CARTESIAN_POINT('Ctrl Pts',(84.6509461975464,53.2632392482302,29.3355096052918)) ;
#15634 = CARTESIAN_POINT('Ctrl Pts',(84.9674095674054,53.2957824613305,29.3144670440925)) ;
#15635 = CARTESIAN_POINT('Ctrl Pts',(85.3014744615188,53.1571613317139,29.2934244828932)) ;
#15636 = CARTESIAN_POINT('Ctrl Pts',(85.5019248616669,52.9101233543463,29.2723819216939)) ;
#15637 = CARTESIAN_POINT('Ctrl Pts',(85.702375261815,52.6630853769787,29.2513393604946)) ;
#15638 = CARTESIAN_POINT('Ctrl Pts',(85.7692111679977,52.3076305518603,29.2302967992953)) ;
#15639 = CARTESIAN_POINT('Ctrl Pts',(85.6721789983957,52.004657148335,29.209254238096)) ;
#15640 = CARTESIAN_POINT('Ctrl Pts',(85.5751468287936,51.7016837448097,29.1882116768967)) ;
#15641 = CARTESIAN_POINT('Ctrl Pts',(85.3142465834066,51.4511917628776,29.1671691156975)) ;
#15642 = CARTESIAN_POINT('Ctrl Pts',(85.0075759640742,51.3665675558227,29.1461265544982)) ;
#15643 = CARTESIAN_POINT('Ctrl Pts',(84.7009053447418,51.2819433487679,29.1250839932989)) ;
#15644 = CARTESIAN_POINT('Ctrl Pts',(84.3484643514639,51.3631869165903,29.1040414320996)) ;
#15645 = CARTESIAN_POINT('Ctrl Pts',(84.1097870286733,51.5735229828435,29.0829988709003)) ;
#15646 = CARTESIAN_POINT('Ctrl Pts',(83.9055712785534,51.7534895462563,29.0649945528968)) ;
#15647 = CARTESIAN_POINT('Ctrl Pts',(83.7846391780019,52.0279616258427,29.0469902348932)) ;
#15648 = CARTESIAN_POINT('Ctrl Pts',(83.782407671779,52.3007005599052,29.0289859168897)) ;
#15649 = CARTESIAN_POINT('Ctrl Pts',(83.782396840654,52.3006964898307,28.9710140831103)) ;
#15650 = CARTESIAN_POINT('Ctrl Pts',(83.7846226433473,52.0275600060296,28.9890451700451)) ;
#15651 = CARTESIAN_POINT('Ctrl Pts',(83.9059573682543,51.7526919543628,29.0070762569799)) ;
#15652 = CARTESIAN_POINT('Ctrl Pts',(84.1107039457943,51.5727159480407,29.0251073439146)) ;
#15653 = CARTESIAN_POINT('Ctrl Pts',(84.3496464124251,51.3626811264497,29.0461499051139)) ;
#15654 = CARTESIAN_POINT('Ctrl Pts',(84.7021896164851,51.2818822106329,29.0671924663132)) ;
#15655 = CARTESIAN_POINT('Ctrl Pts',(85.0087532473587,51.3668932032513,29.0882350275125)) ;
#15656 = CARTESIAN_POINT('Ctrl Pts',(85.3153168782323,51.4519041958698,29.1092775887118)) ;
#15657 = CARTESIAN_POINT('Ctrl Pts',(85.5759009359194,51.7027250969235,29.1303201499111)) ;
#15658 = CARTESIAN_POINT('Ctrl Pts',(85.6725508424044,52.0058206663679,29.1513627111104)) ;
#15659 = CARTESIAN_POINT('Ctrl Pts',(85.7692007488893,52.3089162358123,29.1724052723097)) ;
#15660 = CARTESIAN_POINT('Ctrl Pts',(85.7019165041721,52.6642864736473,29.1934478335089)) ;
#15661 = CARTESIAN_POINT('Ctrl Pts',(85.5011546325818,52.9110713993538,29.2144903947082)) ;
#15662 = CARTESIAN_POINT('Ctrl Pts',(85.3003927609915,53.1578563250602,29.2355329559075)) ;
#15663 = CARTESIAN_POINT('Ctrl Pts',(84.9661532625282,53.296055938638,29.2565755171068)) ;
#15664 = CARTESIAN_POINT('Ctrl Pts',(84.6497311908775,53.2631135463041,29.2776180783061)) ;
#15665 = CARTESIAN_POINT('Ctrl Pts',(84.3333091192268,53.2301711539701,29.2986606395054)) ;
#15666 = CARTESIAN_POINT('Ctrl Pts',(84.0347044743889,53.0260867557244,29.3197032007047)) ;
#15667 = CARTESIAN_POINT('Ctrl Pts',(83.8890820288675,52.7432400976202,29.340745761904)) ;
#15668 = CARTESIAN_POINT('Ctrl Pts',(83.8192593028512,52.6076214116222,29.3508352023061)) ;
#15669 = CARTESIAN_POINT('Ctrl Pts',(83.7846070216412,52.4538953659082,29.3609246427082)) ;
#15670 = CARTESIAN_POINT('Ctrl Pts',(83.784757957323,52.3001050761132,29.3710140831103)) ;
#15671 = CARTESIAN_POINT('Origin',(84.75,52.3,26.4)) ;
#15672 = CARTESIAN_POINT('',(83.7827524248469,52.2992003133627,29.8289859168897)) ;
#15673 = CARTESIAN_POINT('',(83.7827642412961,52.2991978560061,29.7710140831103)) ;
#15674 = CARTESIAN_POINT('',(83.78325,52.3,26.4)) ;
#15675 = CARTESIAN_POINT('Ctrl Pts',(83.7827524248469,52.2992003133627,29.8289859168897)) ;
#15676 = CARTESIAN_POINT('Ctrl Pts',(83.7850677815131,52.5599079824122,29.8117917414187)) ;
#15677 = CARTESIAN_POINT('Ctrl Pts',(83.8942008215872,52.8223250596572,29.7945975659478)) ;
#15678 = CARTESIAN_POINT('Ctrl Pts',(84.0825254981447,53.001512148494,29.7774033904768)) ;
#15679 = CARTESIAN_POINT('Ctrl Pts',(84.3130008436182,53.2208047391355,29.7563608292775)) ;
#15680 = CARTESIAN_POINT('Ctrl Pts',(84.6620841409586,53.3154410037131,29.7353182680783)) ;
#15681 = CARTESIAN_POINT('Ctrl Pts',(84.971761222317,53.2425833996989,29.714275706879)) ;
#15682 = CARTESIAN_POINT('Ctrl Pts',(85.2814383036755,53.1697257956847,29.6932331456797)) ;
#15683 = CARTESIAN_POINT('Ctrl Pts',(85.551709169052,52.9293743230787,29.6721905844804)) ;
#15684 = CARTESIAN_POINT('Ctrl Pts',(85.6602344621622,52.6303251867537,29.6511480232811)) ;
#15685 = CARTESIAN_POINT('Ctrl Pts',(85.7687597552723,52.3312760504287,29.6301054620818)) ;
#15686 = CARTESIAN_POINT('Ctrl Pts',(85.7155394761161,51.9735292503846,29.6090629008825)) ;
#15687 = CARTESIAN_POINT('Ctrl Pts',(85.524664030014,51.7190205290081,29.5880203396832)) ;
#15688 = CARTESIAN_POINT('Ctrl Pts',(85.3337885839119,51.4645118076316,29.566977778484)) ;
#15689 = CARTESIAN_POINT('Ctrl Pts',(85.005257970864,51.3132411649226,29.5459352172847)) ;
#15690 = CARTESIAN_POINT('Ctrl Pts',(84.6877830911888,51.333681956409,29.5248926560854)) ;
#15691 = CARTESIAN_POINT('Ctrl Pts',(84.3703082115136,51.3541227478954,29.5038500948861)) ;
#15692 = CARTESIAN_POINT('Ctrl Pts',(84.063889065211,51.5462749735772,29.4828075336868)) ;
#15693 = CARTESIAN_POINT('Ctrl Pts',(83.9072276949881,51.8231600404575,29.4617649724875)) ;
#15694 = CARTESIAN_POINT('Ctrl Pts',(83.8258812638838,51.9669326372676,29.4508386206216)) ;
#15695 = CARTESIAN_POINT('Ctrl Pts',(83.7849126231147,52.1335509585936,29.4399122687556)) ;
#15696 = CARTESIAN_POINT('Ctrl Pts',(83.7847592665387,52.3000985915647,29.4289859168897)) ;
#15697 = CARTESIAN_POINT('Ctrl Pts',(83.784757957323,52.3001050761132,29.3710140831103)) ;
#15698 = CARTESIAN_POINT('Ctrl Pts',(83.7849218134627,52.1331499671655,29.3819672039075)) ;
#15699 = CARTESIAN_POINT('Ctrl Pts',(83.8261023948951,51.9661191444747,29.3929203247047)) ;
#15700 = CARTESIAN_POINT('Ctrl Pts',(83.9078298636839,51.8220972916435,29.4038734455018)) ;
#15701 = CARTESIAN_POINT('Ctrl Pts',(84.0648403902266,51.5454100617337,29.4249160067011)) ;
#15702 = CARTESIAN_POINT('Ctrl Pts',(84.3715016895169,51.3536445198768,29.4459585679004)) ;
#15703 = CARTESIAN_POINT('Ctrl Pts',(84.689002107179,51.3336042248495,29.4670011290997)) ;
#15704 = CARTESIAN_POINT('Ctrl Pts',(85.006502524841,51.3135639298222,29.488043690299)) ;
#15705 = CARTESIAN_POINT('Ctrl Pts',(85.3348420608748,51.4652488816244,29.5090862514983)) ;
#15706 = CARTESIAN_POINT('Ctrl Pts',(85.5253963068553,51.7199981858024,29.5301288126976)) ;
#15707 = CARTESIAN_POINT('Ctrl Pts',(85.7159505528357,51.9747474899804,29.5511713738969)) ;
#15708 = CARTESIAN_POINT('Ctrl Pts',(85.7687195087629,52.3325611465344,29.5722139350961)) ;
#15709 = CARTESIAN_POINT('Ctrl Pts',(85.6598170628616,52.6314731501694,29.5932564962954)) ;
#15710 = CARTESIAN_POINT('Ctrl Pts',(85.5509146169603,52.9303851538044,29.6142990574947)) ;
#15711 = CARTESIAN_POINT('Ctrl Pts',(85.2803407692306,53.1703955045205,29.635341618694)) ;
#15712 = CARTESIAN_POINT('Ctrl Pts',(84.9705720223194,53.242862407845,29.6563841798933)) ;
#15713 = CARTESIAN_POINT('Ctrl Pts',(84.6608032754083,53.3153293111694,29.6774267410926)) ;
#15714 = CARTESIAN_POINT('Ctrl Pts',(84.3118396293156,53.2202527671022,29.6984693022919)) ;
#15715 = CARTESIAN_POINT('Ctrl Pts',(84.0816410911999,53.0006696127169,29.7195118634912)) ;
#15716 = CARTESIAN_POINT('Ctrl Pts',(83.8938354409632,52.8215244390423,29.7366792700309)) ;
#15717 = CARTESIAN_POINT('Ctrl Pts',(83.7850796413422,52.5595078807163,29.7538466765706)) ;
#15718 = CARTESIAN_POINT('Ctrl Pts',(83.7827642412961,52.2991978560061,29.7710140831103)) ;
#15719 = CARTESIAN_POINT('Origin',(84.75,52.3,26.4)) ;
#15720 = CARTESIAN_POINT('',(83.7824862293435,52.3007282075195,30.2289859168897)) ;
#15721 = CARTESIAN_POINT('',(83.7824750955529,52.3007244933117,30.1710140831103)) ;
#15722 = CARTESIAN_POINT('',(83.78325,52.3,26.4)) ;
#15723 = CARTESIAN_POINT('Ctrl Pts',(83.7824862293435,52.3007282075195,30.2289859168897)) ;
#15724 = CARTESIAN_POINT('Ctrl Pts',(83.782075295683,52.3496619525008,30.2257563364804)) ;
#15725 = CARTESIAN_POINT('Ctrl Pts',(83.7854712604975,52.3985385126902,30.2225267560711)) ;
#15726 = CARTESIAN_POINT('Ctrl Pts',(83.7928735252652,52.4468006010654,30.2192971756619)) ;
#15727 = CARTESIAN_POINT('Ctrl Pts',(83.8411035086217,52.761255675579,30.1982546144626)) ;
#15728 = CARTESIAN_POINT('Ctrl Pts',(84.0594116156069,53.0496247818971,30.1772120532633)) ;
#15729 = CARTESIAN_POINT('Ctrl Pts',(84.3489796726717,53.1813763113338,30.156169492064)) ;
#15730 = CARTESIAN_POINT('Ctrl Pts',(84.6385477297366,53.3131278407706,30.1351269308647)) ;
#15731 = CARTESIAN_POINT('Ctrl Pts',(84.999375736881,53.288261793326,30.1140843696654)) ;
#15732 = CARTESIAN_POINT('Ctrl Pts',(85.2681332290841,53.1180339002943,30.0930418084661)) ;
#15733 = CARTESIAN_POINT('Ctrl Pts',(85.5368907212873,52.9478060072626,30.0719992472669)) ;
#15734 = CARTESIAN_POINT('Ctrl Pts',(85.7135776985492,52.6322162686438,30.0509566860676)) ;
#15735 = CARTESIAN_POINT('Ctrl Pts',(85.7182159840437,52.3141178381398,30.0299141248683)) ;
#15736 = CARTESIAN_POINT('Ctrl Pts',(85.7228542695383,51.9960194076358,30.008871563669)) ;
#15737 = CARTESIAN_POINT('Ctrl Pts',(85.5554438632655,51.6754122852466,29.9878290024697)) ;
#15738 = CARTESIAN_POINT('Ctrl Pts',(85.2917638593211,51.4974207666249,29.9667864412704)) ;
#15739 = CARTESIAN_POINT('Ctrl Pts',(85.0280838553767,51.3194292480032,29.9457438800711)) ;
#15740 = CARTESIAN_POINT('Ctrl Pts',(84.6681342537607,51.284053333149,29.9247013188718)) ;
#15741 = CARTESIAN_POINT('Ctrl Pts',(84.3748479051717,51.407306093413,29.9036587576725)) ;
#15742 = CARTESIAN_POINT('Ctrl Pts',(84.0815615565827,51.530558853677,29.8826161964733)) ;
#15743 = CARTESIAN_POINT('Ctrl Pts',(83.8549384610206,51.8124402890592,29.861573635274)) ;
#15744 = CARTESIAN_POINT('Ctrl Pts',(83.7975606100427,52.125355465103,29.8405310740747)) ;
#15745 = CARTESIAN_POINT('Ctrl Pts',(83.7870670156207,52.1825832087348,29.8366826883464)) ;
#15746 = CARTESIAN_POINT('Ctrl Pts',(83.7822342036874,52.240848944637,29.832834302618)) ;
#15747 = CARTESIAN_POINT('Ctrl Pts',(83.7827524248469,52.2992003133627,29.8289859168897)) ;
#15748 = CARTESIAN_POINT('Ctrl Pts',(83.7827642412961,52.2991978560061,29.7710140831103)) ;
#15749 = CARTESIAN_POINT('Ctrl Pts',(83.7822415919806,52.2404387415845,29.7748892377699)) ;
#15750 = CARTESIAN_POINT('Ctrl Pts',(83.7871423870742,52.1817665799574,29.7787643924295)) ;
#15751 = CARTESIAN_POINT('Ctrl Pts',(83.7977816579324,52.1241541408295,29.782639547089)) ;
#15752 = CARTESIAN_POINT('Ctrl Pts',(83.855554192919,51.8113115880308,29.8036821082883)) ;
#15753 = CARTESIAN_POINT('Ctrl Pts',(84.0825326930308,51.5297162471369,29.8247246694876)) ;
#15754 = CARTESIAN_POINT('Ctrl Pts',(84.3759742911983,51.4068335506118,29.8457672306869)) ;
#15755 = CARTESIAN_POINT('Ctrl Pts',(84.6694158893658,51.2839508540868,29.8668097918862)) ;
#15756 = CARTESIAN_POINT('Ctrl Pts',(85.0293205855891,51.3197808019306,29.8878523530855)) ;
#15757 = CARTESIAN_POINT('Ctrl Pts',(85.2927758558033,51.4981048026616,29.9088949142848)) ;
#15758 = CARTESIAN_POINT('Ctrl Pts',(85.5562311260175,51.6764288033927,29.9299374754841)) ;
#15759 = CARTESIAN_POINT('Ctrl Pts',(85.7232369702226,51.997246857011,29.9509800366833)) ;
#15760 = CARTESIAN_POINT('Ctrl Pts',(85.7181974212124,52.3153391888679,29.9720225978826)) ;
#15761 = CARTESIAN_POINT('Ctrl Pts',(85.7131578722021,52.6334315207248,29.9930651590819)) ;
#15762 = CARTESIAN_POINT('Ctrl Pts',(85.5360729299765,52.9487981308203,30.0141077202812)) ;
#15763 = CARTESIAN_POINT('Ctrl Pts',(85.2671009120418,53.1186868656103,30.0351502814805)) ;
#15764 = CARTESIAN_POINT('Ctrl Pts',(84.9981288941072,53.2885756004003,30.0561928426798)) ;
#15765 = CARTESIAN_POINT('Ctrl Pts',(84.6372698004635,53.3129864598848,30.0772354038791)) ;
#15766 = CARTESIAN_POINT('Ctrl Pts',(84.3478681675789,53.1808697557022,30.0982779650784)) ;
#15767 = CARTESIAN_POINT('Ctrl Pts',(84.0584665346943,53.0487530515197,30.1193205262777)) ;
#15768 = CARTESIAN_POINT('Ctrl Pts',(83.8405223625687,52.76010878367,30.140363087477)) ;
#15769 = CARTESIAN_POINT('Ctrl Pts',(83.7926890879558,52.4455931139805,30.1614056486763)) ;
#15770 = CARTESIAN_POINT('Ctrl Pts',(83.7854085597202,52.397721831233,30.1646084601543)) ;
#15771 = CARTESIAN_POINT('Ctrl Pts',(83.7820689521351,52.3492511915763,30.1678112716323)) ;
#15772 = CARTESIAN_POINT('Ctrl Pts',(83.7824750955529,52.3007244933117,30.1710140831103)) ;
#15773 = CARTESIAN_POINT('Origin',(84.75,52.3,26.4)) ;
#15774 = CARTESIAN_POINT('',(83.7847661033277,52.3000521019819,30.6289859168897)) ;
#15775 = CARTESIAN_POINT('',(83.7847653843543,52.3000586182133,30.5710140831103)) ;
#15776 = CARTESIAN_POINT('',(83.78325,52.3,26.4)) ;
#15777 = CARTESIAN_POINT('Ctrl Pts',(83.7847661033277,52.3000521019819,30.6289859168897)) ;
#15778 = CARTESIAN_POINT('Ctrl Pts',(83.784689680815,52.4571702230074,30.6186783703428)) ;
#15779 = CARTESIAN_POINT('Ctrl Pts',(83.8209307306342,52.6142551143286,30.6083708237959)) ;
#15780 = CARTESIAN_POINT('Ctrl Pts',(83.8936830616376,52.7520650464375,30.5980632772491)) ;
#15781 = CARTESIAN_POINT('Ctrl Pts',(84.0422048626859,53.033400077726,30.5770207160498)) ;
#15782 = CARTESIAN_POINT('Ctrl Pts',(84.3428912751165,53.2344046855717,30.5559781548505)) ;
#15783 = CARTESIAN_POINT('Ctrl Pts',(84.6596352047527,53.2640932054744,30.5349355936512)) ;
#15784 = CARTESIAN_POINT('Ctrl Pts',(84.9763791343889,53.2937817253771,30.5138930324519)) ;
#15785 = CARTESIAN_POINT('Ctrl Pts',(85.3091805812308,53.1521541573367,30.4928504712526)) ;
#15786 = CARTESIAN_POINT('Ctrl Pts',(85.5073954322809,52.9033188744703,30.4718079100534)) ;
#15787 = CARTESIAN_POINT('Ctrl Pts',(85.705610283331,52.6544835916039,30.4507653488541)) ;
#15788 = CARTESIAN_POINT('Ctrl Pts',(85.7692385385893,52.2984405939114,30.4297227876548)) ;
#15789 = CARTESIAN_POINT('Ctrl Pts',(85.6694785742636,51.9963543898182,30.4086802264555)) ;
#15790 = CARTESIAN_POINT('Ctrl Pts',(85.5697186099378,51.694268185725,30.3876376652562)) ;
#15791 = CARTESIAN_POINT('Ctrl Pts',(85.306570426028,51.446138775231,30.3665951040569)) ;
#15792 = CARTESIAN_POINT('Ctrl Pts',(84.999149264129,51.3642830827168,30.3455525428576)) ;
#15793 = CARTESIAN_POINT('Ctrl Pts',(84.6917281022299,51.2824273902026,30.3245099816583)) ;
#15794 = CARTESIAN_POINT('Ctrl Pts',(84.3400339623416,51.3668454156681,30.303467420459)) ;
#15795 = CARTESIAN_POINT('Ctrl Pts',(84.1032628222613,51.5793249497555,30.2824248592598)) ;
#15796 = CARTESIAN_POINT('Ctrl Pts',(83.9028309580058,51.7591934468992,30.2646118784697)) ;
#15797 = CARTESIAN_POINT('Ctrl Pts',(83.7847527632191,52.0308306515281,30.2467988976797)) ;
#15798 = CARTESIAN_POINT('Ctrl Pts',(83.7824862293435,52.3007282075195,30.2289859168897)) ;
#15799 = CARTESIAN_POINT('Ctrl Pts',(83.7824750955529,52.3007244933117,30.1710140831103)) ;
#15800 = CARTESIAN_POINT('Ctrl Pts',(83.7847373257758,52.0304294235648,30.1888538328316)) ;
#15801 = CARTESIAN_POINT('Ctrl Pts',(83.9032122760979,51.7583951236067,30.2066935825528)) ;
#15802 = CARTESIAN_POINT('Ctrl Pts',(84.104172425537,51.5785096804386,30.2245333322741)) ;
#15803 = CARTESIAN_POINT('Ctrl Pts',(84.3412114148312,51.3663289881155,30.2455758934734)) ;
#15804 = CARTESIAN_POINT('Ctrl Pts',(84.69301177052,51.2823546749988,30.2666184546727)) ;
#15805 = CARTESIAN_POINT('Ctrl Pts',(85.0003294357354,51.3645981020112,30.287661015872)) ;
#15806 = CARTESIAN_POINT('Ctrl Pts',(85.3076471009508,51.4468415290236,30.3087035770713)) ;
#15807 = CARTESIAN_POINT('Ctrl Pts',(85.5704820756929,51.6953026961652,30.3297461382705)) ;
#15808 = CARTESIAN_POINT('Ctrl Pts',(85.6698608939394,51.997514507855,30.3507886994698)) ;
#15809 = CARTESIAN_POINT('Ctrl Pts',(85.7692397121858,52.2997263195448,30.3718312606691)) ;
#15810 = CARTESIAN_POINT('Ctrl Pts',(85.7051623739367,52.6556887757828,30.3928738218684)) ;
#15811 = CARTESIAN_POINT('Ctrl Pts',(85.5066337824851,52.9042738256472,30.4139163830677)) ;
#15812 = CARTESIAN_POINT('Ctrl Pts',(85.3081051910334,53.1528588755117,30.434958944267)) ;
#15813 = CARTESIAN_POINT('Ctrl Pts',(84.9751253463793,53.2940665190026,30.4560015054663)) ;
#15814 = CARTESIAN_POINT('Ctrl Pts',(84.6584191140949,53.2639784637058,30.4770440666656)) ;
#15815 = CARTESIAN_POINT('Ctrl Pts',(84.3417128818105,53.233890408409,30.4980866278649)) ;
#15816 = CARTESIAN_POINT('Ctrl Pts',(84.0412802618958,53.0325066543245,30.5191291890641)) ;
#15817 = CARTESIAN_POINT('Ctrl Pts',(83.8931134682116,52.7509844884226,30.5401717502634)) ;
#15818 = CARTESIAN_POINT('Ctrl Pts',(83.8207235228308,52.6134410233427,30.5504525278791)) ;
#15819 = CARTESIAN_POINT('Ctrl Pts',(83.7846796237543,52.456768417478,30.5607333054947)) ;
#15820 = CARTESIAN_POINT('Ctrl Pts',(83.7847653843543,52.3000586182133,30.5710140831103)) ;
#15821 = CARTESIAN_POINT('Origin',(84.75,52.3,26.4)) ;
#15822 = CARTESIAN_POINT('',(83.7826684881877,52.2992194180186,31.0289859168897)) ;
#15823 = CARTESIAN_POINT('',(83.782680142622,52.2992165895442,30.9710140831103)) ;
#15824 = CARTESIAN_POINT('',(83.78325,52.3,26.4)) ;
#15825 = CARTESIAN_POINT('Ctrl Pts',(83.7826684881877,52.2992194180186,31.0289859168897)) ;
#15826 = CARTESIAN_POINT('Ctrl Pts',(83.7849787270906,52.5627690272941,31.0116004042052)) ;
#15827 = CARTESIAN_POINT('Ctrl Pts',(83.8968315418767,52.8280450612531,30.9942148915207)) ;
#15828 = CARTESIAN_POINT('Ctrl Pts',(84.0888777674471,53.007501874752,30.9768293788363)) ;
#15829 = CARTESIAN_POINT('Ctrl Pts',(84.3213209819787,53.2247074900949,30.955786817637)) ;
#15830 = CARTESIAN_POINT('Ctrl Pts',(84.6712433690026,53.3161924146107,30.9347442564377)) ;
#15831 = CARTESIAN_POINT('Ctrl Pts',(84.9802509462634,53.2405455880425,30.9137016952384)) ;
#15832 = CARTESIAN_POINT('Ctrl Pts',(85.2892585235242,53.1648987614744,30.8926591340391)) ;
#15833 = CARTESIAN_POINT('Ctrl Pts',(85.5573512910218,52.9221201838222,30.8716165728398)) ;
#15834 = CARTESIAN_POINT('Ctrl Pts',(85.6631758168593,52.6221046935596,30.8505740116405)) ;
#15835 = CARTESIAN_POINT('Ctrl Pts',(85.7690003426968,52.3220892032969,30.8295314504413)) ;
#15836 = CARTESIAN_POINT('Ctrl Pts',(85.7125566268742,51.9648368004238,30.808488889242)) ;
#15837 = CARTESIAN_POINT('Ctrl Pts',(85.5193941790459,51.7120594394717,30.7874463280427)) ;
#15838 = CARTESIAN_POINT('Ctrl Pts',(85.3262317312177,51.4592820785195,30.7664037668434)) ;
#15839 = CARTESIAN_POINT('Ctrl Pts',(84.9963505513838,51.3109797594882,30.7453612056441)) ;
#15840 = CARTESIAN_POINT('Ctrl Pts',(84.6790728797514,51.3342822108441,30.7243186444448)) ;
#15841 = CARTESIAN_POINT('Ctrl Pts',(84.361795208119,51.3575846622,30.7032760832455)) ;
#15842 = CARTESIAN_POINT('Ctrl Pts',(84.0571210446882,51.552491883943,30.6822335220462)) ;
#15843 = CARTESIAN_POINT('Ctrl Pts',(83.9029625578057,51.8307782221802,30.6611909608469)) ;
#15844 = CARTESIAN_POINT('Ctrl Pts',(83.824317491751,51.9727480085695,30.6504559461945)) ;
#15845 = CARTESIAN_POINT('Ctrl Pts',(83.7848456951869,52.1364180767848,30.6397209315421)) ;
#15846 = CARTESIAN_POINT('Ctrl Pts',(83.7847661033277,52.3000521019819,30.6289859168897)) ;
#15847 = CARTESIAN_POINT('Ctrl Pts',(83.7847653843543,52.3000586182133,30.5710140831103)) ;
#15848 = CARTESIAN_POINT('Ctrl Pts',(83.7848551574291,52.1360168493726,30.581775866694)) ;
#15849 = CARTESIAN_POINT('Ctrl Pts',(83.8245344699275,51.9719343253853,30.5925376502777)) ;
#15850 = CARTESIAN_POINT('Ctrl Pts',(83.9035551198438,51.8297100872491,30.6032994338613)) ;
#15851 = CARTESIAN_POINT('Ctrl Pts',(84.0580645326141,51.5516184296964,30.6243419950606)) ;
#15852 = CARTESIAN_POINT('Ctrl Pts',(84.3629843256084,51.3570956923101,30.6453845562599)) ;
#15853 = CARTESIAN_POINT('Ctrl Pts',(84.6802911452845,51.3341934910749,30.6664271174592)) ;
#15854 = CARTESIAN_POINT('Ctrl Pts',(84.9975979649606,51.3112912898398,30.6874696786584)) ;
#15855 = CARTESIAN_POINT('Ctrl Pts',(85.3272918113186,51.4600096247557,30.7085122398577)) ;
#15856 = CARTESIAN_POINT('Ctrl Pts',(85.5201352411866,51.7130304543972,30.729554801057)) ;
#15857 = CARTESIAN_POINT('Ctrl Pts',(85.7129786710545,51.9660512840388,30.7505973622563)) ;
#15858 = CARTESIAN_POINT('Ctrl Pts',(85.7689716844323,52.323374608406,30.7716399234556)) ;
#15859 = CARTESIAN_POINT('Ctrl Pts',(85.6627687848767,52.6232563729606,30.7926824846549)) ;
#15860 = CARTESIAN_POINT('Ctrl Pts',(85.5565658853211,52.9231381375152,30.8137250458542)) ;
#15861 = CARTESIAN_POINT('Ctrl Pts',(85.288167072832,53.1655783422572,30.8347676070535)) ;
#15862 = CARTESIAN_POINT('Ctrl Pts',(84.9790643106336,53.2408353088181,30.8558101682527)) ;
#15863 = CARTESIAN_POINT('Ctrl Pts',(84.6699615484351,53.3160922753791,30.876852729452)) ;
#15864 = CARTESIAN_POINT('Ctrl Pts',(84.3201548365273,53.224166003759,30.8978952906514)) ;
#15865 = CARTESIAN_POINT('Ctrl Pts',(84.0879857990347,53.006667344109,30.9189378518507)) ;
#15866 = CARTESIAN_POINT('Ctrl Pts',(83.8964614503065,52.8272451025016,30.9362965956039)) ;
#15867 = CARTESIAN_POINT('Ctrl Pts',(83.7849916140278,52.5623686358697,30.9536553393571)) ;
#15868 = CARTESIAN_POINT('Ctrl Pts',(83.782680142622,52.2992165895442,30.9710140831103)) ;
#15869 = CARTESIAN_POINT('Origin',(84.75,52.3,26.4)) ;
#15870 = CARTESIAN_POINT('',(83.7825667404007,52.3007531219363,31.4289859168897)) ;
#15871 = CARTESIAN_POINT('',(83.7825553766487,52.3007499079334,31.3710140831103)) ;
#15872 = CARTESIAN_POINT('',(83.78325,52.3,26.4)) ;
#15873 = CARTESIAN_POINT('Ctrl Pts',(83.7825667404007,52.3007531219363,31.4289859168897)) ;
#15874 = CARTESIAN_POINT('Ctrl Pts',(83.7821217885114,52.3525970280063,31.4255649992669)) ;
#15875 = CARTESIAN_POINT('Ctrl Pts',(83.7859345114109,52.4043754474013,31.4221440816441)) ;
#15876 = CARTESIAN_POINT('Ctrl Pts',(83.7942359163689,52.4554239704382,31.4187231640213)) ;
#15877 = CARTESIAN_POINT('Ctrl Pts',(83.8452990640768,52.7694308506349,31.397680602822)) ;
#15878 = CARTESIAN_POINT('Ctrl Pts',(84.0661986252004,53.0558209430958,31.3766380416228)) ;
#15879 = CARTESIAN_POINT('Ctrl Pts',(84.3569429082262,53.1849565172998,31.3555954804235)) ;
#15880 = CARTESIAN_POINT('Ctrl Pts',(84.6476871912519,53.3140920915038,31.3345529192242)) ;
#15881 = CARTESIAN_POINT('Ctrl Pts',(85.0082761961798,53.2859731474509,31.3135103580249)) ;
#15882 = CARTESIAN_POINT('Ctrl Pts',(85.2754878820815,53.1133288069547,31.2924677968256)) ;
#15883 = CARTESIAN_POINT('Ctrl Pts',(85.5426995679832,52.9406844664586,31.2714252356263)) ;
#15884 = CARTESIAN_POINT('Ctrl Pts',(85.7165339348589,52.6235147295192,31.250382674427)) ;
#15885 = CARTESIAN_POINT('Ctrl Pts',(85.7183039355651,52.3053874743441,31.2293401132277)) ;
#15886 = CARTESIAN_POINT('Ctrl Pts',(85.7200739362713,51.9872602191691,31.2082975520285)) ;
#15887 = CARTESIAN_POINT('Ctrl Pts',(85.5497795708082,51.6681754457583,31.1872549908292)) ;
#15888 = CARTESIAN_POINT('Ctrl Pts',(85.2845054286732,51.4925685825908,31.1662124296299)) ;
#15889 = CARTESIAN_POINT('Ctrl Pts',(85.0192312865381,51.3169617194232,31.1451698684306)) ;
#15890 = CARTESIAN_POINT('Ctrl Pts',(84.6589773677312,51.2848327664989,31.1241273072313)) ;
#15891 = CARTESIAN_POINT('Ctrl Pts',(84.3668142449798,51.4107249289525,31.103084746032)) ;
#15892 = CARTESIAN_POINT('Ctrl Pts',(84.0746511222284,51.5366170914061,31.0820421848327)) ;
#15893 = CARTESIAN_POINT('Ctrl Pts',(83.8505787955325,51.8205303692377,31.0609996236334)) ;
#15894 = CARTESIAN_POINT('Ctrl Pts',(83.7960246532043,52.1339501612384,31.0399570624342)) ;
#15895 = CARTESIAN_POINT('Ctrl Pts',(83.7865435285784,52.1884203074339,31.0363000139193)) ;
#15896 = CARTESIAN_POINT('Ctrl Pts',(83.7821825286476,52.2437816679403,31.0326429654045)) ;
#15897 = CARTESIAN_POINT('Ctrl Pts',(83.7826684881877,52.2992194180186,31.0289859168897)) ;
#15898 = CARTESIAN_POINT('Ctrl Pts',(83.782680142622,52.2992165895442,30.9710140831103)) ;
#15899 = CARTESIAN_POINT('Ctrl Pts',(83.7821896095044,52.2433712983756,30.9746979005564)) ;
#15900 = CARTESIAN_POINT('Ctrl Pts',(83.7866151303081,52.1876036681652,30.9783817180024)) ;
#15901 = CARTESIAN_POINT('Ctrl Pts',(83.7962348619755,52.1327468994487,30.9820655354485)) ;
#15902 = CARTESIAN_POINT('Ctrl Pts',(83.8511843254861,51.8193961621186,31.0031080966478)) ;
#15903 = CARTESIAN_POINT('Ctrl Pts',(84.0756146155844,51.5357657351382,31.0241506578471)) ;
#15904 = CARTESIAN_POINT('Ctrl Pts',(84.3679363214755,51.4102422357509,31.0451932190464)) ;
#15905 = CARTESIAN_POINT('Ctrl Pts',(84.6602580273666,51.2847187363636,31.0662357802457)) ;
#15906 = CARTESIAN_POINT('Ctrl Pts',(85.0204711490505,51.3173021645692,31.0872783414449)) ;
#15907 = CARTESIAN_POINT('Ctrl Pts',(85.2855235578632,51.4932434938774,31.1083209026442)) ;
#15908 = CARTESIAN_POINT('Ctrl Pts',(85.550575966676,51.6691848231856,31.1293634638435)) ;
#15909 = CARTESIAN_POINT('Ctrl Pts',(85.7204676626176,51.9884840535963,31.1504060250428)) ;
#15910 = CARTESIAN_POINT('Ctrl Pts',(85.718296372969,52.3066088866807,31.1714485862421)) ;
#15911 = CARTESIAN_POINT('Ctrl Pts',(85.7161250833204,52.6247337197652,31.1924911474414)) ;
#15912 = CARTESIAN_POINT('Ctrl Pts',(85.5418908080815,52.9416841555234,31.2135337086407)) ;
#15913 = CARTESIAN_POINT('Ctrl Pts',(85.2744615202819,53.113991167422,31.23457626984)) ;
#15914 = CARTESIAN_POINT('Ctrl Pts',(85.0070322324822,53.2862981793206,31.2556188310392)) ;
#15915 = CARTESIAN_POINT('Ctrl Pts',(84.6464079321218,53.3139617673597,31.2766613922386)) ;
#15916 = CARTESIAN_POINT('Ctrl Pts',(84.3558268285061,53.1844597729726,31.2977039534378)) ;
#15917 = CARTESIAN_POINT('Ctrl Pts',(84.0652457248903,53.0549577785855,31.3187465146371)) ;
#15918 = CARTESIAN_POINT('Ctrl Pts',(83.8447078180192,52.7682902017724,31.3397890758364)) ;
#15919 = CARTESIAN_POINT('Ctrl Pts',(83.7940407058406,52.4542186643746,31.3608316370357)) ;
#15920 = CARTESIAN_POINT('Ctrl Pts',(83.7858681402068,52.4035591706175,31.3642257857272)) ;
#15921 = CARTESIAN_POINT('Ctrl Pts',(83.7821151774617,52.3521866960117,31.3676199344188)) ;
#15922 = CARTESIAN_POINT('Ctrl Pts',(83.7825553766487,52.3007499079334,31.3710140831103)) ;
#15923 = CARTESIAN_POINT('Origin',(84.75,52.3,26.4)) ;
#15924 = CARTESIAN_POINT('',(83.7847843561952,52.3000678891362,31.8289859168897)) ;
#15925 = CARTESIAN_POINT('',(83.7847716506988,52.3000190203057,31.7710140831103)) ;
#15926 = CARTESIAN_POINT('',(83.78325,52.3,26.4)) ;
#15927 = CARTESIAN_POINT('Ctrl Pts',(83.7847843561952,52.3000678891362,31.8289859168897)) ;
#15928 = CARTESIAN_POINT('Ctrl Pts',(83.7847679988345,52.4600707944189,31.8184870331293)) ;
#15929 = CARTESIAN_POINT('Ctrl Pts',(83.8224240277508,52.6200556305873,31.8079881493689)) ;
#15930 = CARTESIAN_POINT('Ctrl Pts',(83.8977846402365,52.7597306844102,31.7974892656085)) ;
#15931 = CARTESIAN_POINT('Ctrl Pts',(84.0488273926318,53.0396767182138,31.7764467044092)) ;
#15932 = CARTESIAN_POINT('Ctrl Pts',(84.3513326348141,53.2380366447095,31.75540414321)) ;
#15933 = CARTESIAN_POINT('Ctrl Pts',(84.668336119238,53.264886980438,31.7343615820107)) ;
#15934 = CARTESIAN_POINT('Ctrl Pts',(84.9853396036619,53.2917373161665,31.7133190208114)) ;
#15935 = CARTESIAN_POINT('Ctrl Pts',(85.3168413303273,53.1470780611279,31.6922764596121)) ;
#15936 = CARTESIAN_POINT('Ctrl Pts',(85.5128021802699,52.8964563788972,31.6712338984128)) ;
#15937 = CARTESIAN_POINT('Ctrl Pts',(85.7087630302126,52.6458346966665,31.6501913372135)) ;
#15938 = CARTESIAN_POINT('Ctrl Pts',(85.7691830034324,52.2892505872438,31.6291487760142)) ;
#15939 = CARTESIAN_POINT('Ctrl Pts',(85.666704506489,51.9880807358278,31.608106214815)) ;
#15940 = CARTESIAN_POINT('Ctrl Pts',(85.5642260095456,51.6869108844117,31.5870636536157)) ;
#15941 = CARTESIAN_POINT('Ctrl Pts',(85.298849042439,51.4411552910024,31.5660210924164)) ;
#15942 = CARTESIAN_POINT('Ctrl Pts',(84.9907017630098,51.3620725037616,31.5449785312171)) ;
#15943 = CARTESIAN_POINT('Ctrl Pts',(84.6825544835806,51.2829897165209,31.5239359700178)) ;
#15944 = CARTESIAN_POINT('Ctrl Pts',(84.3316368918287,51.3705797354487,31.5028934088185)) ;
#15945 = CARTESIAN_POINT('Ctrl Pts',(84.0967914630988,51.5851865788789,31.4818508476192)) ;
#15946 = CARTESIAN_POINT('Ctrl Pts',(83.9001251732181,51.7649044976337,31.4642292040427)) ;
#15947 = CARTESIAN_POINT('Ctrl Pts',(83.7848587522135,52.0336976312407,31.4466075604662)) ;
#15948 = CARTESIAN_POINT('Ctrl Pts',(83.7825667404007,52.3007531219363,31.4289859168897)) ;
#15949 = CARTESIAN_POINT('Ctrl Pts',(83.7825553766487,52.3007499079334,31.3710140831103)) ;
#15950 = CARTESIAN_POINT('Ctrl Pts',(83.7848442618873,52.0332961996321,31.388662495618)) ;
#15951 = CARTESIAN_POINT('Ctrl Pts',(83.900501333443,51.7641036837555,31.4063109081258)) ;
#15952 = CARTESIAN_POINT('Ctrl Pts',(84.097693462439,51.5843621896236,31.4239593206336)) ;
#15953 = CARTESIAN_POINT('Ctrl Pts',(84.3328096487019,51.3700527502527,31.4450018818329)) ;
#15954 = CARTESIAN_POINT('Ctrl Pts',(84.6838383387137,51.2829093694934,31.4660444430321)) ;
#15955 = CARTESIAN_POINT('Ctrl Pts',(84.9918851656152,51.3623788006393,31.4870870042314)) ;
#15956 = CARTESIAN_POINT('Ctrl Pts',(85.2999319925168,51.4418482317852,31.5081295654307)) ;
#15957 = CARTESIAN_POINT('Ctrl Pts',(85.5649969563081,51.6879304748365,31.52917212663)) ;
#15958 = CARTESIAN_POINT('Ctrl Pts',(85.6670963806458,51.9892334402438,31.5502146878293)) ;
#15959 = CARTESIAN_POINT('Ctrl Pts',(85.7691958049835,52.2905364056511,31.5712572490286)) ;
#15960 = CARTESIAN_POINT('Ctrl Pts',(85.7083296898676,52.6470600934144,31.5922998102279)) ;
#15961 = CARTESIAN_POINT('Ctrl Pts',(85.5120509779309,52.8974261121282,31.6133423714272)) ;
#15962 = CARTESIAN_POINT('Ctrl Pts',(85.3157722659941,53.1477921308421,31.6343849326264)) ;
#15963 = CARTESIAN_POINT('Ctrl Pts',(84.9840809572364,53.2920004805065,31.6554274938257)) ;
#15964 = CARTESIAN_POINT('Ctrl Pts',(84.6671153793743,53.2647670691806,31.676470055025)) ;
#15965 = CARTESIAN_POINT('Ctrl Pts',(84.3501498015122,53.2375336578548,31.6975126162243)) ;
#15966 = CARTESIAN_POINT('Ctrl Pts',(84.0479099545456,53.0388584855388,31.7185551774236)) ;
#15967 = CARTESIAN_POINT('Ctrl Pts',(83.8972127505983,52.7586880401527,31.7395977386229)) ;
#15968 = CARTESIAN_POINT('Ctrl Pts',(83.8222162513974,52.619257433392,31.750069853452)) ;
#15969 = CARTESIAN_POINT('Ctrl Pts',(83.7847521621177,52.4596429764979,31.7605419682812)) ;
#15970 = CARTESIAN_POINT('Ctrl Pts',(83.7847716506988,52.3000190203057,31.7710140831103)) ;
#15971 = CARTESIAN_POINT('Origin',(84.75,52.3,25.7604774406976)) ;
#15972 = CARTESIAN_POINT('',(84.012172416957,52.3000518747697,31.9604774406976)) ;
#15973 = CARTESIAN_POINT('',(84.0115563622989,52.2999794994122,32.0395225593024)) ;
#15974 = CARTESIAN_POINT('',(84.011,52.2999999999999,25.7604774406976)) ;
#15975 = CARTESIAN_POINT('',(84.6290678012582,51.5698174568242,32.05)) ;
#15976 = CARTESIAN_POINT('Ctrl Pts',(84.0121728877458,52.3000518956002,31.9604774406976)) ;
#15977 = CARTESIAN_POINT('Ctrl Pts',(84.012185444936,52.1772211438289,31.9710211181365)) ;
#15978 = CARTESIAN_POINT('Ctrl Pts',(84.0944207311608,51.8295445255366,32.0008619712373)) ;
#15979 = CARTESIAN_POINT('Ctrl Pts',(84.4090991301214,51.6076008033498,32.0307028243381)) ;
#15980 = CARTESIAN_POINT('Ctrl Pts',(84.6290682970003,51.5698134220425,32.05)) ;
#15981 = CARTESIAN_POINT('',(84.0209858286879,52.1789242467453,32.05)) ;
#15982 = CARTESIAN_POINT('Origin',(84.75,52.3,32.05)) ;
#15983 = CARTESIAN_POINT('Ctrl Pts',(84.0115565511623,52.299979492453,32.0395225593024)) ;
#15984 = CARTESIAN_POINT('Ctrl Pts',(84.0112610663628,52.2594454132586,32.0430150395349)) ;
#15985 = CARTESIAN_POINT('Ctrl Pts',(84.0143436429872,52.2189177828097,32.0465075197675)) ;
#15986 = CARTESIAN_POINT('Ctrl Pts',(84.0209858286879,52.1789242467453,32.05)) ;
#15987 = CARTESIAN_POINT('Origin',(84.75,52.3,25.7604774406976)) ;
#15988 = CARTESIAN_POINT('',(84.0104777048421,52.3005756991061,31.5604774406976)) ;
#15989 = CARTESIAN_POINT('',(84.0121631754502,52.3000145394422,31.6395225593024)) ;
#15990 = CARTESIAN_POINT('',(84.011,52.2999999999999,25.7604774406976)) ;
#15991 = CARTESIAN_POINT('Ctrl Pts',(84.0104777048421,52.3005756991061,31.5604774406976)) ;
#15992 = CARTESIAN_POINT('Ctrl Pts',(84.0122297573166,52.0964339792985,31.5780990842741)) ;
#15993 = CARTESIAN_POINT('Ctrl Pts',(84.2055581925249,51.6456057548941,31.6167632890499)) ;
#15994 = CARTESIAN_POINT('Ctrl Pts',(84.9666908338978,51.4556249045992,31.676470055025)) ;
#15995 = CARTESIAN_POINT('Ctrl Pts',(85.5752667181236,52.0192040621772,31.7395977386228)) ;
#15996 = CARTESIAN_POINT('Ctrl Pts',(85.4367085793821,52.836940778588,31.8027254222208)) ;
#15997 = CARTESIAN_POINT('Ctrl Pts',(84.6764920518234,53.1686806993748,31.8658531058186)) ;
#15998 = CARTESIAN_POINT('Ctrl Pts',(84.0986379054398,52.7897679070709,31.9184371119776)) ;
#15999 = CARTESIAN_POINT('Ctrl Pts',(84.0121603839034,52.4223608141459,31.9499785569372)) ;
#16000 = CARTESIAN_POINT('Ctrl Pts',(84.0121728877458,52.3000518956002,31.9604774406976)) ;
#16001 = CARTESIAN_POINT('Ctrl Pts',(84.0121631754502,52.3000145394422,31.6395225593024)) ;
#16002 = CARTESIAN_POINT('Ctrl Pts',(84.0121782127345,52.1768495541185,31.6500930056725)) ;
#16003 = CARTESIAN_POINT('Ctrl Pts',(84.09953271401,51.8084782135297,31.681706013242)) ;
#16004 = CARTESIAN_POINT('Ctrl Pts',(84.6793843110363,51.4310793972544,31.7343615820107)) ;
#16005 = CARTESIAN_POINT('Ctrl Pts',(85.4385697001617,51.7654585545426,31.7974892656085)) ;
#16006 = CARTESIAN_POINT('Ctrl Pts',(85.5742157004875,52.583371203896,31.8606169492065)) ;
#16007 = CARTESIAN_POINT('Ctrl Pts',(84.9640410903861,53.1455422795452,31.9237446328042)) ;
#16008 = CARTESIAN_POINT('Ctrl Pts',(84.203885152176,52.9519357106028,31.9833798361696)) ;
#16009 = CARTESIAN_POINT('Ctrl Pts',(84.0130413933977,52.5036675091086,32.0219724783357)) ;
#16010 = CARTESIAN_POINT('Ctrl Pts',(84.0115565511623,52.299979492453,32.0395225593024)) ;
#16011 = CARTESIAN_POINT('Origin',(84.75,52.3,25.7604774406976)) ;
#16012 = CARTESIAN_POINT('',(84.010555482566,52.2994033099723,31.1604774406976)) ;
#16013 = CARTESIAN_POINT('',(84.0104690181984,52.3005732422681,31.2395225593024)) ;
#16014 = CARTESIAN_POINT('',(84.011,52.2999999999999,25.7604774406976)) ;
#16015 = CARTESIAN_POINT('Ctrl Pts',(84.010555482566,52.2994033099723,31.1604774406976)) ;
#16016 = CARTESIAN_POINT('Ctrl Pts',(84.0101840069,52.2570257590979,31.1641344892124)) ;
#16017 = CARTESIAN_POINT('Ctrl Pts',(84.0326992015831,51.9712032804197,31.1888340989266)) ;
#16018 = CARTESIAN_POINT('Ctrl Pts',(84.4050365955573,51.4994291370381,31.2345762698399)) ;
#16019 = CARTESIAN_POINT('Ctrl Pts',(85.2311891044738,51.5731088770259,31.2977039534378)) ;
#16020 = CARTESIAN_POINT('Ctrl Pts',(85.6217167571572,52.3048502193085,31.3608316370357)) ;
#16021 = CARTESIAN_POINT('Ctrl Pts',(85.2230709941749,53.0321999030888,31.4239593206336)) ;
#16022 = CARTESIAN_POINT('Ctrl Pts',(84.3961500488167,53.0966836878991,31.4870870042314)) ;
#16023 = CARTESIAN_POINT('Ctrl Pts',(84.0309796581042,52.6232505066463,31.5325930442528)) ;
#16024 = CARTESIAN_POINT('Ctrl Pts',(84.0101375761158,52.3402060550262,31.5570565230748)) ;
#16025 = CARTESIAN_POINT('Ctrl Pts',(84.0104777048421,52.3005756991061,31.5604774406976)) ;
#16026 = CARTESIAN_POINT('Ctrl Pts',(84.0104690181984,52.3005732422681,31.2395225593024)) ;
#16027 = CARTESIAN_POINT('Ctrl Pts',(84.0122186806669,52.0961271182085,31.2571709718101)) ;
#16028 = CARTESIAN_POINT('Ctrl Pts',(84.2060421944615,51.6450017472081,31.2958619455172)) ;
#16029 = CARTESIAN_POINT('Ctrl Pts',(84.9677571597911,51.4559049037231,31.3555954804235)) ;
#16030 = CARTESIAN_POINT('Ctrl Pts',(85.5756175422327,52.0202331507826,31.4187231640214)) ;
#16031 = CARTESIAN_POINT('Ctrl Pts',(85.4360362883285,52.8378313051878,31.4818508476192)) ;
#16032 = CARTESIAN_POINT('Ctrl Pts',(84.6753850015265,53.1685371869628,31.5449785312171)) ;
#16033 = CARTESIAN_POINT('Ctrl Pts',(84.0983317306906,52.7892154027258,31.5975357684448)) ;
#16034 = CARTESIAN_POINT('Ctrl Pts',(84.0121482780501,52.4220337829137,31.6290504444732)) ;
#16035 = CARTESIAN_POINT('Ctrl Pts',(84.0121631754502,52.3000145394422,31.6395225593024)) ;
#16036 = CARTESIAN_POINT('Origin',(84.75,52.3,25.7604774406976)) ;
#16037 = CARTESIAN_POINT('',(84.0121589349461,52.3000398276334,30.7604774406976)) ;
#16038 = CARTESIAN_POINT('',(84.0105643914121,52.2994011478387,30.8395225593024)) ;
#16039 = CARTESIAN_POINT('',(84.011,52.2999999999999,25.7604774406976)) ;
#16040 = CARTESIAN_POINT('Ctrl Pts',(84.0121589349461,52.3000398276334,30.7604774406976)) ;
#16041 = CARTESIAN_POINT('Ctrl Pts',(84.0122197763053,52.1749552198024,30.77121245535)) ;
#16042 = CARTESIAN_POINT('Ctrl Pts',(84.1015370120932,51.8046007047638,30.8029900312018)) ;
#16043 = CARTESIAN_POINT('Ctrl Pts',(84.6861477792349,51.4306114595269,30.8558101682528)) ;
#16044 = CARTESIAN_POINT('Ctrl Pts',(85.4426479868293,51.7707058389346,30.9189378518506)) ;
#16045 = CARTESIAN_POINT('Ctrl Pts',(85.5720875709808,52.5899751196893,30.9820655354485)) ;
#16046 = CARTESIAN_POINT('Ctrl Pts',(84.9572836759283,53.14672723415,31.0451932190464)) ;
#16047 = CARTESIAN_POINT('Ctrl Pts',(84.2013112353611,52.9490831729925,31.1046638541294)) ;
#16048 = CARTESIAN_POINT('Ctrl Pts',(84.0123214681354,52.5008650749111,31.1430919280131)) ;
#16049 = CARTESIAN_POINT('Ctrl Pts',(84.010555482566,52.2994033099723,31.1604774406976)) ;
#16050 = CARTESIAN_POINT('Ctrl Pts',(84.0105643914121,52.2994011478387,30.8395225593024)) ;
#16051 = CARTESIAN_POINT('Ctrl Pts',(84.0101894196264,52.2567120656835,30.8432063767484)) ;
#16052 = CARTESIAN_POINT('Ctrl Pts',(84.0328962784322,51.9705745100615,30.8679327553938)) ;
#16053 = CARTESIAN_POINT('Ctrl Pts',(84.406046739384,51.4989945619123,30.9137016952384)) ;
#16054 = CARTESIAN_POINT('Ctrl Pts',(85.2321056902744,51.5737165276034,30.9768293788363)) ;
#16055 = CARTESIAN_POINT('Ctrl Pts',(85.6217099208433,52.3059496735259,31.0399570624342)) ;
#16056 = CARTESIAN_POINT('Ctrl Pts',(85.2221470677742,53.0327964447449,31.103084746032)) ;
#16057 = CARTESIAN_POINT('Ctrl Pts',(84.3951451811447,53.0962359841114,31.1662124296299)) ;
#16058 = CARTESIAN_POINT('Ctrl Pts',(84.0307871030694,52.6226228587488,31.21169170072)) ;
#16059 = CARTESIAN_POINT('Ctrl Pts',(84.0101325225179,52.339892390331,31.2361284106108)) ;
#16060 = CARTESIAN_POINT('Ctrl Pts',(84.0104690181984,52.3005732422681,31.2395225593024)) ;
#16061 = CARTESIAN_POINT('Origin',(84.75,52.3,25.7604774406976)) ;
#16062 = CARTESIAN_POINT('',(84.0104161608325,52.3005566541059,30.3604774406976)) ;
#16063 = CARTESIAN_POINT('',(84.0121583853507,52.3000448087505,30.4395225593024)) ;
#16064 = CARTESIAN_POINT('',(84.011,52.2999999999999,25.7604774406976)) ;
#16065 = CARTESIAN_POINT('Ctrl Pts',(84.0104161608325,52.3005566541059,30.3604774406976)) ;
#16066 = CARTESIAN_POINT('Ctrl Pts',(84.0121487375422,52.0942424116672,30.3782904214876)) ;
#16067 = CARTESIAN_POINT('Ctrl Pts',(84.2090354168613,51.6413074113017,30.4171459634769)) ;
#16068 = CARTESIAN_POINT('Ctrl Pts',(84.9742969091548,51.4576197781646,30.4770440666656)) ;
#16069 = CARTESIAN_POINT('Ctrl Pts',(85.5777616350177,52.0266426931532,30.5401717502634)) ;
#16070 = CARTESIAN_POINT('Ctrl Pts',(85.4318461016247,52.8431385047737,30.6032994338613)) ;
#16071 = CARTESIAN_POINT('Ctrl Pts',(84.6686489900153,53.1679260075878,30.6664271174592)) ;
#16072 = CARTESIAN_POINT('Ctrl Pts',(84.096359217492,52.7853584004575,30.7188197864046)) ;
#16073 = CARTESIAN_POINT('Ctrl Pts',(84.0121005162889,52.4201435684535,30.7501698941507)) ;
#16074 = CARTESIAN_POINT('Ctrl Pts',(84.0121589349461,52.3000398276334,30.7604774406976)) ;
#16075 = CARTESIAN_POINT('Ctrl Pts',(84.0121583853507,52.3000448087505,30.4395225593024)) ;
#16076 = CARTESIAN_POINT('Ctrl Pts',(84.0122270094027,52.1746485148035,30.450284342886)) ;
#16077 = CARTESIAN_POINT('Ctrl Pts',(84.1018659252076,51.8039722448119,30.482088687669)) ;
#16078 = CARTESIAN_POINT('Ctrl Pts',(84.6872445240728,51.4305315890238,30.5349355936513)) ;
#16079 = CARTESIAN_POINT('Ctrl Pts',(85.4433151290645,51.7715799971008,30.5980632772491)) ;
#16080 = CARTESIAN_POINT('Ctrl Pts',(85.5717211395724,52.5910119186134,30.661190960847)) ;
#16081 = CARTESIAN_POINT('Ctrl Pts',(84.9562154066652,53.1469880592007,30.7243186444448)) ;
#16082 = CARTESIAN_POINT('Ctrl Pts',(84.2008330365987,52.9484799043716,30.7837625105966)) ;
#16083 = CARTESIAN_POINT('Ctrl Pts',(84.0123313191275,52.5005590089554,30.8221638155492)) ;
#16084 = CARTESIAN_POINT('Ctrl Pts',(84.0105643914121,52.2994011478387,30.8395225593024)) ;
#16085 = CARTESIAN_POINT('Origin',(84.75,52.3,25.7604774406976)) ;
#16086 = CARTESIAN_POINT('',(84.0106196451636,52.2993887060512,29.9604774406976)) ;
#16087 = CARTESIAN_POINT('',(84.0104076499753,52.3005538149027,30.0395225593024)) ;
#16088 = CARTESIAN_POINT('',(84.011,52.2999999999999,25.7604774406976)) ;
#16089 = CARTESIAN_POINT('Ctrl Pts',(84.0106196451636,52.2993887060512,29.9604774406976)) ;
#16090 = CARTESIAN_POINT('Ctrl Pts',(84.0102235081717,52.2547839359573,29.9643258264259)) ;
#16091 = CARTESIAN_POINT('Ctrl Pts',(84.0341177346705,51.9667084407867,29.9892167733536)) ;
#16092 = CARTESIAN_POINT('Ctrl Pts',(84.4122688988207,51.4963512925987,30.0351502814805)) ;
#16093 = CARTESIAN_POINT('Ctrl Pts',(85.237723532162,51.5774771299215,30.0982779650784)) ;
#16094 = CARTESIAN_POINT('Ctrl Pts',(85.6216375437542,52.3127095998846,30.1614056486762)) ;
#16095 = CARTESIAN_POINT('Ctrl Pts',(85.2164500303437,53.036435951597,30.2245333322741)) ;
#16096 = CARTESIAN_POINT('Ctrl Pts',(84.3889809930133,53.0934600293675,30.2876610158719)) ;
#16097 = CARTESIAN_POINT('Ctrl Pts',(84.029611953797,52.6187597073854,30.3329757186798)) ;
#16098 = CARTESIAN_POINT('Ctrl Pts',(84.0101020362138,52.3379624338227,30.3572478602883)) ;
#16099 = CARTESIAN_POINT('Ctrl Pts',(84.0104161608325,52.3005566541059,30.3604774406976)) ;
#16100 = CARTESIAN_POINT('Ctrl Pts',(84.0104076499753,52.3005538149027,30.0395225593024)) ;
#16101 = CARTESIAN_POINT('Ctrl Pts',(84.0121369369003,52.093935706247,30.0573623090236)) ;
#16102 = CARTESIAN_POINT('Ctrl Pts',(84.2095246450093,51.6407071811469,30.0962446199442)) ;
#16103 = CARTESIAN_POINT('Ctrl Pts',(84.975359359988,51.4579033746375,30.156169492064)) ;
#16104 = CARTESIAN_POINT('Ctrl Pts',(85.5781058187447,52.0276870907513,30.2192971756619)) ;
#16105 = CARTESIAN_POINT('Ctrl Pts',(85.4311604255217,52.8439982006345,30.2824248592598)) ;
#16106 = CARTESIAN_POINT('Ctrl Pts',(84.6675542030255,53.1678227112312,30.3455525428576)) ;
#16107 = CARTESIAN_POINT('Ctrl Pts',(84.0960396207762,52.7847293170448,30.3979184428719)) ;
#16108 = CARTESIAN_POINT('Ctrl Pts',(84.0120928285021,52.4198364215321,30.4292417816868)) ;
#16109 = CARTESIAN_POINT('Ctrl Pts',(84.0121583853507,52.3000448087505,30.4395225593024)) ;
#16110 = CARTESIAN_POINT('Origin',(84.75,52.3,25.7604774406976)) ;
#16111 = CARTESIAN_POINT('',(84.0121537087894,52.3000753650543,29.5604774406976)) ;
#16112 = CARTESIAN_POINT('',(84.0106286778565,52.2993868276063,29.6395225593024)) ;
#16113 = CARTESIAN_POINT('',(84.011,52.2999999999999,25.7604774406976)) ;
#16114 = CARTESIAN_POINT('Ctrl Pts',(84.0121537087894,52.3000753650543,29.5604774406976)) ;
#16115 = CARTESIAN_POINT('Ctrl Pts',(84.0122709371417,52.1727635463156,29.5714037925636)) ;
#16116 = CARTESIAN_POINT('Ctrl Pts',(84.1039002651515,51.8001096205179,29.6033727056288)) ;
#16117 = CARTESIAN_POINT('Ctrl Pts',(84.6939891568927,51.4300710793027,29.6563841798933)) ;
#16118 = CARTESIAN_POINT('Ctrl Pts',(85.4473921764194,51.7769725687113,29.7195118634912)) ;
#16119 = CARTESIAN_POINT('Ctrl Pts',(85.5694396125602,52.5973756260661,29.7826395470891)) ;
#16120 = CARTESIAN_POINT('Ctrl Pts',(84.9496407932796,53.1485617804674,29.8457672306869)) ;
#16121 = CARTESIAN_POINT('Ctrl Pts',(84.1979075099158,52.9447673553597,29.9050465285564)) ;
#16122 = CARTESIAN_POINT('Ctrl Pts',(84.0123895428375,52.4986780439644,29.9432832652267)) ;
#16123 = CARTESIAN_POINT('Ctrl Pts',(84.0106196451636,52.2993887060512,29.9604774406976)) ;
#16124 = CARTESIAN_POINT('Ctrl Pts',(84.0106286778565,52.2993868276063,29.6395225593024)) ;
#16125 = CARTESIAN_POINT('Ctrl Pts',(84.0102291559076,52.2544703698276,29.6433977139619)) ;
#16126 = CARTESIAN_POINT('Ctrl Pts',(84.0343180016969,51.9660794808919,29.6683154298208)) ;
#16127 = CARTESIAN_POINT('Ctrl Pts',(84.4132829291257,51.4959258854032,29.714275706879)) ;
#16128 = CARTESIAN_POINT('Ctrl Pts',(85.2386345831491,51.5780929341436,29.7774033904768)) ;
#16129 = CARTESIAN_POINT('Ctrl Pts',(85.6216208325441,52.3138091222706,29.8405310740747)) ;
#16130 = CARTESIAN_POINT('Ctrl Pts',(85.2155206857491,53.0370237843669,29.9036587576725)) ;
#16131 = CARTESIAN_POINT('Ctrl Pts',(84.3879803592861,53.0930040020832,29.9667864412704)) ;
#16132 = CARTESIAN_POINT('Ctrl Pts',(84.0294223509248,52.6181314106496,30.012074375147)) ;
#16133 = CARTESIAN_POINT('Ctrl Pts',(84.0100971870989,52.3376484412462,30.0363197478244)) ;
#16134 = CARTESIAN_POINT('Ctrl Pts',(84.0104076499753,52.3005538149027,30.0395225593024)) ;
#16135 = CARTESIAN_POINT('Origin',(84.75,52.3,25.7604774406976)) ;
#16136 = CARTESIAN_POINT('',(84.0103561101056,52.3005355198033,29.1604774406976)) ;
#16137 = CARTESIAN_POINT('',(84.0121527080028,52.3000803219525,29.2395225593024)) ;
#16138 = CARTESIAN_POINT('',(84.011,52.2999999999999,25.7604774406976)) ;
#16139 = CARTESIAN_POINT('Ctrl Pts',(84.0103561101056,52.3005355198033,29.1604774406976)) ;
#16140 = CARTESIAN_POINT('Ctrl Pts',(84.012061911087,52.0920492800597,29.1784817587012)) ;
#16141 = CARTESIAN_POINT('Ctrl Pts',(84.2125467370667,51.6370213192352,29.217528637904)) ;
#16142 = CARTESIAN_POINT('Ctrl Pts',(84.9818830553883,51.4596763776764,29.2776180783061)) ;
#16143 = CARTESIAN_POINT('Ctrl Pts',(85.5801926949256,52.0341172609902,29.340745761904)) ;
#16144 = CARTESIAN_POINT('Ctrl Pts',(85.4269212141838,52.8492642455131,29.4038734455019)) ;
#16145 = CARTESIAN_POINT('Ctrl Pts',(84.6608267013838,53.1671572316628,29.4670011290997)) ;
#16146 = CARTESIAN_POINT('Ctrl Pts',(84.0940868976613,52.780861082125,29.5192024608316)) ;
#16147 = CARTESIAN_POINT('Ctrl Pts',(84.0120451724208,52.4179475537566,29.5503612313643)) ;
#16148 = CARTESIAN_POINT('Ctrl Pts',(84.0121537087894,52.3000753650543,29.5604774406976)) ;
#16149 = CARTESIAN_POINT('Ctrl Pts',(84.0121527080028,52.3000803219525,29.2395225593024)) ;
#16150 = CARTESIAN_POINT('Ctrl Pts',(84.0122779623987,52.172457021707,29.2504756800996)) ;
#16151 = CARTESIAN_POINT('Ctrl Pts',(84.1042331481866,51.7994814638448,29.282471362096)) ;
#16152 = CARTESIAN_POINT('Ctrl Pts',(84.6950865774281,51.4300011013776,29.3355096052917)) ;
#16153 = CARTESIAN_POINT('Ctrl Pts',(85.4480514094807,51.7778527053553,29.3986372888896)) ;
#16154 = CARTESIAN_POINT('Ctrl Pts',(85.5690638483639,52.5984090814401,29.4617649724875)) ;
#16155 = CARTESIAN_POINT('Ctrl Pts',(84.9485702146255,53.148812957869,29.5248926560853)) ;
#16156 = CARTESIAN_POINT('Ctrl Pts',(84.1974339403033,52.9441628692833,29.5841451850237)) ;
#16157 = CARTESIAN_POINT('Ctrl Pts',(84.0123986086908,52.4983721994821,29.6223551527627)) ;
#16158 = CARTESIAN_POINT('Ctrl Pts',(84.0106286778565,52.2993868276063,29.6395225593024)) ;
#16159 = CARTESIAN_POINT('Origin',(84.75,52.3,25.7604774406976)) ;
#16160 = CARTESIAN_POINT('',(84.0106846088523,52.2993761801769,28.7604774406976)) ;
#16161 = CARTESIAN_POINT('',(84.0103478306111,52.3005324085697,28.8395225593024)) ;
#16162 = CARTESIAN_POINT('',(84.011,52.2999999999999,25.7604774406976)) ;
#16163 = CARTESIAN_POINT('Ctrl Pts',(84.0106846088524,52.2993761801769,28.7604774406976)) ;
#16164 = CARTESIAN_POINT('Ctrl Pts',(84.0102646767194,52.2525430796879,28.7645171636395)) ;
#16165 = CARTESIAN_POINT('Ctrl Pts',(84.0355591348416,51.962212287757,28.7895994477806)) ;
#16166 = CARTESIAN_POINT('Ctrl Pts',(84.4195286707959,51.4933388306201,28.835724293121)) ;
#16167 = CARTESIAN_POINT('Ctrl Pts',(85.2442182847965,51.5819040255063,28.8988519767189)) ;
#16168 = CARTESIAN_POINT('Ctrl Pts',(85.6214875174565,52.3205681435423,28.9619796603168)) ;
#16169 = CARTESIAN_POINT('Ctrl Pts',(85.2097910453075,53.0406117311157,29.0251073439146)) ;
#16170 = CARTESIAN_POINT('Ctrl Pts',(84.3818414899421,53.090172672954,29.0882350275125)) ;
#16171 = CARTESIAN_POINT('Ctrl Pts',(84.0282664307177,52.6142693996754,29.1333583931068)) ;
#16172 = CARTESIAN_POINT('Ctrl Pts',(84.0100682548131,52.3357177410451,29.1574391975019)) ;
#16173 = CARTESIAN_POINT('Ctrl Pts',(84.0103561101056,52.3005355198033,29.1604774406976)) ;
#16174 = CARTESIAN_POINT('Ctrl Pts',(84.0103478306111,52.3005324085697,28.8395225593024)) ;
#16175 = CARTESIAN_POINT('Ctrl Pts',(84.0120492717183,52.091742275103,28.8575536462372)) ;
#16176 = CARTESIAN_POINT('Ctrl Pts',(84.2130406468208,51.6364224339068,28.8966272943712)) ;
#16177 = CARTESIAN_POINT('Ctrl Pts',(84.9829429060078,51.4599695421454,28.9567435037046)) ;
#16178 = CARTESIAN_POINT('Ctrl Pts',(85.5805274479185,52.0351647194261,29.0198711873024)) ;
#16179 = CARTESIAN_POINT('Ctrl Pts',(85.4262278145717,52.8501177241122,29.0829988709003)) ;
#16180 = CARTESIAN_POINT('Ctrl Pts',(84.6597328902445,53.1670440683605,29.1461265544982)) ;
#16181 = CARTESIAN_POINT('Ctrl Pts',(84.0937711983123,52.7802317621059,29.1983011172988)) ;
#16182 = CARTESIAN_POINT('Ctrl Pts',(84.0120373302227,52.4176402124707,29.2294331189003)) ;
#16183 = CARTESIAN_POINT('Ctrl Pts',(84.0121527080028,52.3000803219525,29.2395225593024)) ;
#16184 = CARTESIAN_POINT('Origin',(84.75,52.3,25.7604774406976)) ;
#16185 = CARTESIAN_POINT('',(84.012145263812,52.3001106858399,28.3604774406976)) ;
#16186 = CARTESIAN_POINT('',(84.0106937367584,52.299374595264,28.4395225593024)) ;
#16187 = CARTESIAN_POINT('',(84.011,52.2999999999999,25.7604774406976)) ;
#16188 = CARTESIAN_POINT('Ctrl Pts',(84.012145263812,52.3001106858399,28.3604774406976)) ;
#16189 = CARTESIAN_POINT('Ctrl Pts',(84.012320562902,52.1705731480788,28.3715951297771)) ;
#16190 = CARTESIAN_POINT('Ctrl Pts',(84.1062919598857,51.7956207689212,28.4037553800558)) ;
#16191 = CARTESIAN_POINT('Ctrl Pts',(84.7018350882737,51.4296014229731,28.4569581915339)) ;
#16192 = CARTESIAN_POINT('Ctrl Pts',(85.4520796692884,51.7832818180256,28.5200858751317)) ;
#16193 = CARTESIAN_POINT('Ctrl Pts',(85.566725036296,52.6047519593021,28.5832135587296)) ;
#16194 = CARTESIAN_POINT('Ctrl Pts',(84.9419816788649,53.1503273349667,28.6463412423274)) ;
#16195 = CARTESIAN_POINT('Ctrl Pts',(84.1945368090908,52.9404428849206,28.7054292029835)) ;
#16196 = CARTESIAN_POINT('Ctrl Pts',(84.0124520662344,52.4964925775559,28.7434746024402)) ;
#16197 = CARTESIAN_POINT('Ctrl Pts',(84.0106846088524,52.2993761801769,28.7604774406976)) ;
#16198 = CARTESIAN_POINT('Ctrl Pts',(84.0106937367584,52.299374595264,28.4395225593024)) ;
#16199 = CARTESIAN_POINT('Ctrl Pts',(84.0102705539735,52.2522296530489,28.4435890511755)) ;
#16200 = CARTESIAN_POINT('Ctrl Pts',(84.0357626124065,51.9615831483613,28.4686981042478)) ;
#16201 = CARTESIAN_POINT('Ctrl Pts',(84.4205464955366,51.4929225836516,28.5148497185195)) ;
#16202 = CARTESIAN_POINT('Ctrl Pts',(85.2451237463938,51.5825280191257,28.5779774021174)) ;
#16203 = CARTESIAN_POINT('Ctrl Pts',(85.6214608931572,52.3216674705582,28.6411050857152)) ;
#16204 = CARTESIAN_POINT('Ctrl Pts',(85.2088564383358,53.0411911606195,28.7042327693131)) ;
#16205 = CARTESIAN_POINT('Ctrl Pts',(84.3808450086281,53.08970764206,28.767360452911)) ;
#16206 = CARTESIAN_POINT('Ctrl Pts',(84.0280799537887,52.6136413086296,28.8124570495741)) ;
#16207 = CARTESIAN_POINT('Ctrl Pts',(84.0100636632658,52.3354036349076,28.8365110850379)) ;
#16208 = CARTESIAN_POINT('Ctrl Pts',(84.0103478306111,52.3005324085697,28.8395225593024)) ;
#16209 = CARTESIAN_POINT('Origin',(84.75,52.3,25.7604774406976)) ;
#16210 = CARTESIAN_POINT('',(84.0102978130501,52.3005124640715,27.9604774406976)) ;
#16211 = CARTESIAN_POINT('',(84.0121438140165,52.3001156043131,28.0395225593024)) ;
#16212 = CARTESIAN_POINT('',(84.011,52.2999999999999,25.7604774406976)) ;
#16213 = CARTESIAN_POINT('Ctrl Pts',(84.0102978130501,52.3005124640715,27.9604774406976)) ;
#16214 = CARTESIAN_POINT('Ctrl Pts',(84.0119690402742,52.0898539400114,27.9786730959147)) ;
#16215 = CARTESIAN_POINT('Ctrl Pts',(84.2160915677973,51.6327449502991,28.017911312331)) ;
#16216 = CARTESIAN_POINT('Ctrl Pts',(84.989450350052,51.4618012935295,28.0781920899466)) ;
#16217 = CARTESIAN_POINT('Ctrl Pts',(85.5825562620867,52.0416134444791,28.1413197735445)) ;
#16218 = CARTESIAN_POINT('Ctrl Pts',(85.4219412946177,52.8553453323684,28.2044474571424)) ;
#16219 = CARTESIAN_POINT('Ctrl Pts',(84.6530116623168,53.1663179577801,28.2675751407402)) ;
#16220 = CARTESIAN_POINT('Ctrl Pts',(84.0918423690182,52.7763621308894,28.3195851352587)) ;
#16221 = CARTESIAN_POINT('Ctrl Pts',(84.011988772563,52.4157501400294,28.3505525685778)) ;
#16222 = CARTESIAN_POINT('Ctrl Pts',(84.012145263812,52.3001106858399,28.3604774406976)) ;
#16223 = CARTESIAN_POINT('Ctrl Pts',(84.0121438140165,52.3001156043131,28.0395225593024)) ;
#16224 = CARTESIAN_POINT('Ctrl Pts',(84.0123273641732,52.1702667990095,28.0506670173131)) ;
#16225 = CARTESIAN_POINT('Ctrl Pts',(84.1066288342844,51.794992936399,28.0828540365231)) ;
#16226 = CARTESIAN_POINT('Ctrl Pts',(84.7029330951489,51.4295413427059,28.1360836169323)) ;
#16227 = CARTESIAN_POINT('Ctrl Pts',(85.4527309398621,51.7841678628247,28.1992113005302)) ;
#16228 = CARTESIAN_POINT('Ctrl Pts',(85.5663399692938,52.6057819846142,28.2623389841281)) ;
#16229 = CARTESIAN_POINT('Ctrl Pts',(84.9409088790051,53.1505688493595,28.3254666677259)) ;
#16230 = CARTESIAN_POINT('Ctrl Pts',(84.1940678498118,52.9398372061532,28.3845278594507)) ;
#16231 = CARTESIAN_POINT('Ctrl Pts',(84.0124603652231,52.4961869417292,28.4225464899762)) ;
#16232 = CARTESIAN_POINT('Ctrl Pts',(84.0106937367584,52.299374595264,28.4395225593024)) ;
#16233 = CARTESIAN_POINT('Origin',(84.75,52.3,25.7604774406976)) ;
#16234 = CARTESIAN_POINT('',(84.0107501619265,52.299365759712,27.5604774406976)) ;
#16235 = CARTESIAN_POINT('',(84.0102897973284,52.3005090881678,27.6395225593024)) ;
#16236 = CARTESIAN_POINT('',(84.011,52.2999999999999,25.7604774406976)) ;
#16237 = CARTESIAN_POINT('Ctrl Pts',(84.0107501619265,52.299365759712,27.5604774406976)) ;
#16238 = CARTESIAN_POINT('Ctrl Pts',(84.0103074630672,52.2503032365772,27.564708500853)) ;
#16239 = CARTESIAN_POINT('Ctrl Pts',(84.0370235408122,51.9577148666482,27.5899821222076)) ;
#16240 = CARTESIAN_POINT('Ctrl Pts',(84.4268153114771,51.490391953806,27.6362983047616)) ;
#16241 = CARTESIAN_POINT('Ctrl Pts',(85.2506728575663,51.5863892979384,27.6994259883594)) ;
#16242 = CARTESIAN_POINT('Ctrl Pts',(85.6212666417578,52.3284250163863,27.7625536719573)) ;
#16243 = CARTESIAN_POINT('Ctrl Pts',(85.203094680064,53.0447272999564,27.8256813555552)) ;
#16244 = CARTESIAN_POINT('Ctrl Pts',(84.3747319174341,53.0868210776482,27.8888090391531)) ;
#16245 = CARTESIAN_POINT('Ctrl Pts',(84.0269431929634,52.6097805786841,27.9337410675339)) ;
#16246 = CARTESIAN_POINT('Ctrl Pts',(84.0100363315741,52.3334722561318,27.9576305347154)) ;
#16247 = CARTESIAN_POINT('Ctrl Pts',(84.0102978130501,52.3005124640715,27.9604774406976)) ;
#16248 = CARTESIAN_POINT('Ctrl Pts',(84.0102897973284,52.3005090881678,27.6395225593024)) ;
#16249 = CARTESIAN_POINT('Ctrl Pts',(84.0119555459036,52.0895466130168,27.6577449834507)) ;
#16250 = CARTESIAN_POINT('Ctrl Pts',(84.2165901750469,51.6321474461671,27.6970099687983)) ;
#16251 = CARTESIAN_POINT('Ctrl Pts',(84.9905075141293,51.4621040018937,27.7573175153451)) ;
#16252 = CARTESIAN_POINT('Ctrl Pts',(85.5828815572153,52.042663878742,27.820445198943)) ;
#16253 = CARTESIAN_POINT('Ctrl Pts',(85.4212402278205,52.8561925242217,27.8835728825408)) ;
#16254 = CARTESIAN_POINT('Ctrl Pts',(84.6519189159883,53.1661949368354,27.9467005661387)) ;
#16255 = CARTESIAN_POINT('Ctrl Pts',(84.0915305454382,52.7757325930713,27.9986837917259)) ;
#16256 = CARTESIAN_POINT('Ctrl Pts',(84.011980791428,52.4154426011558,28.0296244561138)) ;
#16257 = CARTESIAN_POINT('Ctrl Pts',(84.0121438140165,52.3001156043131,28.0395225593024)) ;
#16258 = CARTESIAN_POINT('Origin',(84.75,52.3,25.7604774406976)) ;
#16259 = CARTESIAN_POINT('',(84.0121337603747,52.3001460493381,27.1604774406976)) ;
#16260 = CARTESIAN_POINT('',(84.0107593547378,52.2993644693424,27.2395225593024)) ;
#16261 = CARTESIAN_POINT('',(84.011,52.2999999999999,25.7604774406976)) ;
#16262 = CARTESIAN_POINT('Ctrl Pts',(84.0121337603747,52.3001460493381,27.1604774406976)) ;
#16263 = CARTESIAN_POINT('Ctrl Pts',(84.0123686127965,52.1683841800178,27.1717864669906)) ;
#16264 = CARTESIAN_POINT('Ctrl Pts',(84.1087120145737,51.7911337021563,27.2041380544828)) ;
#16265 = CARTESIAN_POINT('Ctrl Pts',(84.7096850855178,51.4292029103844,27.2575322031744)) ;
#16266 = CARTESIAN_POINT('Ctrl Pts',(85.4567100107038,51.7896328869262,27.3206598867723)) ;
#16267 = CARTESIAN_POINT('Ctrl Pts',(85.5639440986358,52.6121036097496,27.3837875703701)) ;
#16268 = CARTESIAN_POINT('Ctrl Pts',(84.934306938815,53.1520237140672,27.446915253968)) ;
#16269 = CARTESIAN_POINT('Ctrl Pts',(84.1911990172918,52.9361100119052,27.5058118774105)) ;
#16270 = CARTESIAN_POINT('Ctrl Pts',(84.012509161341,52.4943085467702,27.5436659396537)) ;
#16271 = CARTESIAN_POINT('Ctrl Pts',(84.0107501619265,52.299365759712,27.5604774406976)) ;
#16272 = CARTESIAN_POINT('Ctrl Pts',(84.0107593547378,52.2993644693424,27.2395225593024)) ;
#16273 = CARTESIAN_POINT('Ctrl Pts',(84.010313557306,52.2499899466507,27.243780388389)) ;
#16274 = CARTESIAN_POINT('Ctrl Pts',(84.0372302203536,51.95708550979,27.2690807786749)) ;
#16275 = CARTESIAN_POINT('Ctrl Pts',(84.4278368710099,51.4899849375734,27.31542373016)) ;
#16276 = CARTESIAN_POINT('Ctrl Pts',(85.2515726447776,51.5870214121571,27.3785514137579)) ;
#16277 = CARTESIAN_POINT('Ctrl Pts',(85.6212301121436,52.3295240675631,27.4416790973558)) ;
#16278 = CARTESIAN_POINT('Ctrl Pts',(85.2021548839321,53.0452982747,27.5048067809536)) ;
#16279 = CARTESIAN_POINT('Ctrl Pts',(84.3737396709075,53.0863470831135,27.5679344645515)) ;
#16280 = CARTESIAN_POINT('Ctrl Pts',(84.0267598229767,52.6091526983306,27.6128397240011)) ;
#16281 = CARTESIAN_POINT('Ctrl Pts',(84.0100320029078,52.3331580424289,27.6367024222514)) ;
#16282 = CARTESIAN_POINT('Ctrl Pts',(84.0102897973284,52.3005090881678,27.6395225593024)) ;
#16283 = CARTESIAN_POINT('Origin',(84.75,52.3,25.7604774406976)) ;
#16284 = CARTESIAN_POINT('',(84.010254873815,52.3005215753354,26.7604774406976)) ;
#16285 = CARTESIAN_POINT('',(84.0121333942101,52.3001533432303,26.8395225593024)) ;
#16286 = CARTESIAN_POINT('',(84.011,52.2999999999999,25.7604774406976)) ;
#16287 = CARTESIAN_POINT('Ctrl Pts',(84.010254873815,52.3005215753354,26.7604774406976)) ;
#16288 = CARTESIAN_POINT('Ctrl Pts',(84.0118865417744,52.0876983314931,26.7788644331282)) ;
#16289 = CARTESIAN_POINT('Ctrl Pts',(84.2196500716081,51.6284277708823,26.818293986758)) ;
#16290 = CARTESIAN_POINT('Ctrl Pts',(84.9970086663633,51.464021058011,26.8787661015872)) ;
#16291 = CARTESIAN_POINT('Ctrl Pts',(85.584846975971,52.0491174747966,26.941893785185)) ;
#16292 = CARTESIAN_POINT('Ctrl Pts',(85.4169092945958,52.8613877554865,27.0050214687829)) ;
#16293 = CARTESIAN_POINT('Ctrl Pts',(84.6452032531813,53.1654050588536,27.0681491523808)) ;
#16294 = CARTESIAN_POINT('Ctrl Pts',(84.0896257601006,52.7718624007159,27.1199678096857)) ;
#16295 = CARTESIAN_POINT('Ctrl Pts',(84.0119316258861,52.4135518122329,27.1507439057913)) ;
#16296 = CARTESIAN_POINT('Ctrl Pts',(84.0121337603747,52.3001460493381,27.1604774406976)) ;
#16297 = CARTESIAN_POINT('Ctrl Pts',(84.0121333942101,52.3001533432303,26.8395225593024)) ;
#16298 = CARTESIAN_POINT('Ctrl Pts',(84.0123759877409,52.1680792935557,26.8508583545266)) ;
#16299 = CARTESIAN_POINT('Ctrl Pts',(84.1090503779434,51.7905022090762,26.8832367109501)) ;
#16300 = CARTESIAN_POINT('Ctrl Pts',(84.710785203412,51.4291552942847,26.9366576285728)) ;
#16301 = CARTESIAN_POINT('Ctrl Pts',(85.4573524705639,51.7905235055957,26.9997853121707)) ;
#16302 = CARTESIAN_POINT('Ctrl Pts',(85.5635501520105,52.6131307432408,27.0629129957686)) ;
#16303 = CARTESIAN_POINT('Ctrl Pts',(84.933231811866,53.1522552393336,27.1260406793665)) ;
#16304 = CARTESIAN_POINT('Ctrl Pts',(84.1907347271212,52.9355032943271,27.1849105338777)) ;
#16305 = CARTESIAN_POINT('Ctrl Pts',(84.0125167269381,52.4940031266761,27.2227378271897)) ;
#16306 = CARTESIAN_POINT('Ctrl Pts',(84.0107593547378,52.2993644693424,27.2395225593024)) ;
#16307 = CARTESIAN_POINT('Origin',(84.75,52.3,32.05)) ;
#16308 = CARTESIAN_POINT('',(85.6645587247976,52.6133494876276,32.05)) ;
#16309 = CARTESIAN_POINT('Ctrl Pts',(84.6290682970003,51.5698134220425,32.05)) ;
#16310 = CARTESIAN_POINT('Ctrl Pts',(84.6486054756756,51.5633636415286,32.05)) ;
#16311 = CARTESIAN_POINT('Ctrl Pts',(84.6683837217373,51.5577953863303,32.05)) ;
#16312 = CARTESIAN_POINT('Ctrl Pts',(84.6883526700962,51.5531398112781,32.05)) ;
#16313 = CARTESIAN_POINT('Ctrl Pts',(84.7208023354277,51.5455744728509,32.05)) ;
#16314 = CARTESIAN_POINT('Ctrl Pts',(84.7537544638827,51.5404164732051,32.05)) ;
#16315 = CARTESIAN_POINT('Ctrl Pts',(84.7869911094308,51.5375362654893,32.05)) ;
#16316 = CARTESIAN_POINT('Ctrl Pts',(84.797421598867,51.5366323843767,32.05)) ;
#16317 = CARTESIAN_POINT('Ctrl Pts',(84.8078802856998,51.5359531478234,32.05)) ;
#16318 = CARTESIAN_POINT('Ctrl Pts',(84.818360849627,51.5354954119729,32.05)) ;
#16319 = CARTESIAN_POINT('Ctrl Pts',(84.8273128543076,51.5351044355423,32.05)) ;
#16320 = CARTESIAN_POINT('Ctrl Pts',(84.8362803076888,51.5348752539893,32.05)) ;
#16321 = CARTESIAN_POINT('Ctrl Pts',(84.8452455423231,51.5348057051637,32.05)) ;
#16322 = CARTESIAN_POINT('Ctrl Pts',(84.8809024636672,51.5345290925477,32.05)) ;
#16323 = CARTESIAN_POINT('Ctrl Pts',(84.9165773339652,51.5367708227219,32.05)) ;
#16324 = CARTESIAN_POINT('Ctrl Pts',(84.9520181276991,51.5413821237009,32.05)) ;
#16325 = CARTESIAN_POINT('Ctrl Pts',(84.9775637855138,51.5447059408189,32.05)) ;
#16326 = CARTESIAN_POINT('Ctrl Pts',(85.0029885312786,51.5492619056144,32.05)) ;
#16327 = CARTESIAN_POINT('Ctrl Pts',(85.0282030317967,51.5550099525335,32.05)) ;
#16328 = CARTESIAN_POINT('Ctrl Pts',(85.0362872843134,51.5568528866316,32.05)) ;
#16329 = CARTESIAN_POINT('Ctrl Pts',(85.0443485937157,51.5588182817752,32.05)) ;
#16330 = CARTESIAN_POINT('Ctrl Pts',(85.052372137682,51.5609014997111,32.05)) ;
#16331 = CARTESIAN_POINT('Ctrl Pts',(85.0889237057945,51.5703916804338,32.05)) ;
#16332 = CARTESIAN_POINT('Ctrl Pts',(85.1247567909586,51.5823375166551,32.05)) ;
#16333 = CARTESIAN_POINT('Ctrl Pts',(85.1596013391966,51.5965816118641,32.05)) ;
#16334 = CARTESIAN_POINT('Ctrl Pts',(85.1947214437706,51.6109383516871,32.05)) ;
#16335 = CARTESIAN_POINT('Ctrl Pts',(85.2288386803151,51.627629956059,32.05)) ;
#16336 = CARTESIAN_POINT('Ctrl Pts',(85.2616821666479,51.646548385543,32.05)) ;
#16337 = CARTESIAN_POINT('Ctrl Pts',(85.2787824571817,51.6563984555794,32.05)) ;
#16338 = CARTESIAN_POINT('Ctrl Pts',(85.2955374178107,51.6668530503173,32.05)) ;
#16339 = CARTESIAN_POINT('Ctrl Pts',(85.3119074772461,51.677902377199,32.05)) ;
#16340 = CARTESIAN_POINT('Ctrl Pts',(85.3200219818723,51.6833794381989,32.05)) ;
#16341 = CARTESIAN_POINT('Ctrl Pts',(85.3280442877998,51.6890046707409,32.05)) ;
#16342 = CARTESIAN_POINT('Ctrl Pts',(85.3359493062664,51.694761862387,32.05)) ;
#16343 = CARTESIAN_POINT('Ctrl Pts',(85.3685071062967,51.7184735709857,32.05)) ;
#16344 = CARTESIAN_POINT('Ctrl Pts',(85.3991472042605,51.7444650511667,32.05)) ;
#16345 = CARTESIAN_POINT('Ctrl Pts',(85.4275676556062,51.7725897979014,32.05)) ;
#16346 = CARTESIAN_POINT('Ctrl Pts',(85.4543169662164,51.799060791521,32.05)) ;
#16347 = CARTESIAN_POINT('Ctrl Pts',(85.4791015982827,51.8274219759074,32.05)) ;
#16348 = CARTESIAN_POINT('Ctrl Pts',(85.5019075504341,51.8574120322123,32.05)) ;
#16349 = CARTESIAN_POINT('Ctrl Pts',(85.5123316294908,51.8711198009458,32.05)) ;
#16350 = CARTESIAN_POINT('Ctrl Pts',(85.5223419418911,51.8851684883569,32.05)) ;
#16351 = CARTESIAN_POINT('Ctrl Pts',(85.5319350286684,51.8995359094532,32.05)) ;
#16352 = CARTESIAN_POINT('Ctrl Pts',(85.5372176410402,51.9074475981717,32.05)) ;
#16353 = CARTESIAN_POINT('Ctrl Pts',(85.542373710439,51.9154559659869,32.05)) ;
#16354 = CARTESIAN_POINT('Ctrl Pts',(85.5474024643045,51.9235574931787,32.05)) ;
#16355 = CARTESIAN_POINT('Ctrl Pts',(85.5517120936517,51.9305004814967,32.05)) ;
#16356 = CARTESIAN_POINT('Ctrl Pts',(85.5559234083183,51.9375042085288,32.05)) ;
#16357 = CARTESIAN_POINT('Ctrl Pts',(85.5600348116964,51.9445630629369,32.05)) ;
#16358 = CARTESIAN_POINT('Ctrl Pts',(85.5799659198025,51.9787827143242,32.05)) ;
#16359 = CARTESIAN_POINT('Ctrl Pts',(85.5975643889103,52.0143151477684,32.05)) ;
#16360 = CARTESIAN_POINT('Ctrl Pts',(85.6128251657119,52.050862155833,32.05)) ;
#16361 = CARTESIAN_POINT('Ctrl Pts',(85.6284402685273,52.0882577154394,32.05)) ;
#16362 = CARTESIAN_POINT('Ctrl Pts',(85.6416085142695,52.1267164034934,32.05)) ;
#16363 = CARTESIAN_POINT('Ctrl Pts',(85.6522878131956,52.165959075351,32.05)) ;
#16364 = CARTESIAN_POINT('Ctrl Pts',(85.6574156485319,52.184802068775,32.05)) ;
#16365 = CARTESIAN_POINT('Ctrl Pts',(85.6619690371714,52.2038263204532,32.05)) ;
#16366 = CARTESIAN_POINT('Ctrl Pts',(85.6659397311219,52.2230031348788,32.05)) ;
#16367 = CARTESIAN_POINT('Ctrl Pts',(85.6677315738388,52.2316569963174,32.05)) ;
#16368 = CARTESIAN_POINT('Ctrl Pts',(85.6694047219091,52.2403419407282,32.05)) ;
#16369 = CARTESIAN_POINT('Ctrl Pts',(85.6709582458612,52.2490553928039,32.05)) ;
#16370 = CARTESIAN_POINT('Ctrl Pts',(85.6723899282023,52.2570854559705,32.05)) ;
#16371 = CARTESIAN_POINT('Ctrl Pts',(85.6737182376174,52.2651298209158,32.05)) ;
#16372 = CARTESIAN_POINT('Ctrl Pts',(85.6749429936691,52.2731853280596,32.05)) ;
#16373 = CARTESIAN_POINT('Ctrl Pts',(85.6813033393252,52.3150188097536,32.05)) ;
#16374 = CARTESIAN_POINT('Ctrl Pts',(85.6848756544714,52.3571575210195,32.05)) ;
#16375 = CARTESIAN_POINT('Ctrl Pts',(85.6856310209224,52.3992957021883,32.05)) ;
#16376 = CARTESIAN_POINT('Ctrl Pts',(85.6863812796774,52.441148950098,32.05)) ;
#16377 = CARTESIAN_POINT('Ctrl Pts',(85.6843530088631,52.4830028899044,32.05)) ;
#16378 = CARTESIAN_POINT('Ctrl Pts',(85.6794724997026,52.5245795220203,32.05)) ;
#16379 = CARTESIAN_POINT('Ctrl Pts',(85.6759784989651,52.5543446097399,32.05)) ;
#16380 = CARTESIAN_POINT('Ctrl Pts',(85.6710217340403,52.5839680712491,32.05)) ;
#16381 = CARTESIAN_POINT('Ctrl Pts',(85.6645587247976,52.6133494876276,32.05)) ;
#16382 = CARTESIAN_POINT('',(83.78325,52.3,32.05)) ;
#16383 = CARTESIAN_POINT('Origin',(84.75,52.3,32.05)) ;
#16384 = CARTESIAN_POINT('',(85.0634162962529,53.2161025497301,32.05)) ;
#16385 = CARTESIAN_POINT('Origin',(84.75,52.3,32.05)) ;
#16386 = CARTESIAN_POINT('Ctrl Pts',(85.0634162962528,53.2161025497302,32.05)) ;
#16387 = CARTESIAN_POINT('Ctrl Pts',(85.0375903626687,53.2219158833822,32.05)) ;
#16388 = CARTESIAN_POINT('Ctrl Pts',(85.0115585907843,53.2265873685398,32.05)) ;
#16389 = CARTESIAN_POINT('Ctrl Pts',(84.9853698812676,53.2300642668749,32.05)) ;
#16390 = CARTESIAN_POINT('Ctrl Pts',(84.9482204181441,53.2349963505426,32.05)) ;
#16391 = CARTESIAN_POINT('Ctrl Pts',(84.9107544993145,53.2375257569857,32.05)) ;
#16392 = CARTESIAN_POINT('Ctrl Pts',(84.8731799721622,53.2377230918043,32.05)) ;
#16393 = CARTESIAN_POINT('Ctrl Pts',(84.8583111944688,53.2378011800139,32.05)) ;
#16394 = CARTESIAN_POINT('Ctrl Pts',(84.8434255126426,53.2375137512002,32.05)) ;
#16395 = CARTESIAN_POINT('Ctrl Pts',(84.8285363533114,53.2368639235865,32.05)) ;
#16396 = CARTESIAN_POINT('Ctrl Pts',(84.8151276070541,53.2362787076325,32.05)) ;
#16397 = CARTESIAN_POINT('Ctrl Pts',(84.8017114154886,53.2353989415351,32.05)) ;
#16398 = CARTESIAN_POINT('Ctrl Pts',(84.7883268826021,53.234229649649,32.05)) ;
#16399 = CARTESIAN_POINT('Ctrl Pts',(84.7467495586251,53.2305973953159,32.05)) ;
#16400 = CARTESIAN_POINT('Ctrl Pts',(84.7054263758008,53.2241747289076,32.05)) ;
#16401 = CARTESIAN_POINT('Ctrl Pts',(84.6646494982219,53.2150591487198,32.05)) ;
#16402 = CARTESIAN_POINT('Ctrl Pts',(84.6409788399251,53.2097676257633,32.05)) ;
#16403 = CARTESIAN_POINT('Ctrl Pts',(84.6174926209232,53.2035677546806,32.05)) ;
#16404 = CARTESIAN_POINT('Ctrl Pts',(84.5942525737568,53.1964719333739,32.05)) ;
#16405 = CARTESIAN_POINT('Ctrl Pts',(84.585513077665,53.1938035264583,32.05)) ;
#16406 = CARTESIAN_POINT('Ctrl Pts',(84.5768084370589,53.1910083729646,32.05)) ;
#16407 = CARTESIAN_POINT('Ctrl Pts',(84.568142102793,53.188086977312,32.05)) ;
#16408 = CARTESIAN_POINT('Ctrl Pts',(84.5599799601992,53.1853355431811,32.05)) ;
#16409 = CARTESIAN_POINT('Ctrl Pts',(84.5518564838162,53.1824736325861,32.05)) ;
#16410 = CARTESIAN_POINT('Ctrl Pts',(84.5437817785724,53.1795048835846,32.05)) ;
#16411 = CARTESIAN_POINT('Ctrl Pts',(84.5061169942788,53.1656570355968,32.05)) ;
#16412 = CARTESIAN_POINT('Ctrl Pts',(84.469460386035,53.1494709330162,32.05)) ;
#16413 = CARTESIAN_POINT('Ctrl Pts',(84.4340761666869,53.1310298954467,32.05)) ;
#16414 = CARTESIAN_POINT('Ctrl Pts',(84.3995110501093,53.1130157460563,32.05)) ;
#16415 = CARTESIAN_POINT('Ctrl Pts',(84.3661592694239,53.0928491386052,32.05)) ;
#16416 = CARTESIAN_POINT('Ctrl Pts',(84.3343026524149,53.070575118304,32.05)) ;
#16417 = CARTESIAN_POINT('Ctrl Pts',(84.3189936953075,53.0598711561945,32.05)) ;
#16418 = CARTESIAN_POINT('Ctrl Pts',(84.3040306344131,53.0486800927604,32.05)) ;
#16419 = CARTESIAN_POINT('Ctrl Pts',(84.2894485931079,53.0370048640332,32.05)) ;
#16420 = CARTESIAN_POINT('Ctrl Pts',(84.2821858372867,53.0311898801343,32.05)) ;
#16421 = CARTESIAN_POINT('Ctrl Pts',(84.2750176419556,53.0252547731509,32.05)) ;
#16422 = CARTESIAN_POINT('Ctrl Pts',(84.2679486148627,53.019199805017,32.05)) ;
#16423 = CARTESIAN_POINT('Ctrl Pts',(84.2621177465606,53.0142053805654,32.05)) ;
#16424 = CARTESIAN_POINT('Ctrl Pts',(84.2563618671862,53.0091358377593,32.05)) ;
#16425 = CARTESIAN_POINT('Ctrl Pts',(84.2506831552877,53.0039919568579,32.05)) ;
#16426 = CARTESIAN_POINT('Ctrl Pts',(84.2235295101632,52.97939568942,32.05)) ;
#16427 = CARTESIAN_POINT('Ctrl Pts',(84.1981352605778,52.9531001772539,32.05)) ;
#16428 = CARTESIAN_POINT('Ctrl Pts',(84.1747348706618,52.9251520670723,32.05)) ;
#16429 = CARTESIAN_POINT('Ctrl Pts',(84.152837480384,52.8989990551623,32.05)) ;
#16430 = CARTESIAN_POINT('Ctrl Pts',(84.1326864154153,52.8713977926676,32.05)) ;
#16431 = CARTESIAN_POINT('Ctrl Pts',(84.1143384424733,52.8425442600233,32.05)) ;
#16432 = CARTESIAN_POINT('Ctrl Pts',(84.1045838240468,52.8272044073818,32.05)) ;
#16433 = CARTESIAN_POINT('Ctrl Pts',(84.0953393822899,52.8115104725868,32.05)) ;
#16434 = CARTESIAN_POINT('Ctrl Pts',(84.0866173651522,52.7954916943026,32.05)) ;
#16435 = CARTESIAN_POINT('Ctrl Pts',(84.0822883255137,52.7875410190106,32.05)) ;
#16436 = CARTESIAN_POINT('Ctrl Pts',(84.0780880245306,52.7795103220941,32.05)) ;
#16437 = CARTESIAN_POINT('Ctrl Pts',(84.0740181996644,52.7714032163815,32.05)) ;
#16438 = CARTESIAN_POINT('Ctrl Pts',(84.0705530522315,52.764500630282,32.05)) ;
#16439 = CARTESIAN_POINT('Ctrl Pts',(84.0671826623095,52.7575426978405,32.05)) ;
#16440 = CARTESIAN_POINT('Ctrl Pts',(84.0639137672541,52.7505445638357,32.05)) ;
#16441 = CARTESIAN_POINT('Ctrl Pts',(84.0481282892796,52.7167506095102,32.05)) ;
#16442 = CARTESIAN_POINT('Ctrl Pts',(84.0346671737874,52.68194532237,32.05)) ;
#16443 = CARTESIAN_POINT('Ctrl Pts',(84.0235884717775,52.6463938282192,32.05)) ;
#16444 = CARTESIAN_POINT('Ctrl Pts',(84.012629449038,52.6112263841922,32.05)) ;
#16445 = CARTESIAN_POINT('Ctrl Pts',(84.0040017040798,52.5753274496591,32.05)) ;
#16446 = CARTESIAN_POINT('Ctrl Pts',(83.9978116824037,52.5389572210107,32.05)) ;
#16447 = CARTESIAN_POINT('Ctrl Pts',(83.9950331653952,52.5226317048508,32.05)) ;
#16448 = CARTESIAN_POINT('Ctrl Pts',(83.9927464851397,52.506211397335,32.05)) ;
#16449 = CARTESIAN_POINT('Ctrl Pts',(83.9909645624641,52.4897211182932,32.05)) ;
#16450 = CARTESIAN_POINT('Ctrl Pts',(83.9901106015459,52.4818183882679,32.05)) ;
#16451 = CARTESIAN_POINT('Ctrl Pts',(83.9893724702862,52.4738979582126,32.05)) ;
#16452 = CARTESIAN_POINT('Ctrl Pts',(83.9887521538462,52.4659678151963,32.05)) ;
#16453 = CARTESIAN_POINT('Ctrl Pts',(83.9859881691425,52.4306329561157,32.05)) ;
#16454 = CARTESIAN_POINT('Ctrl Pts',(83.9855712457582,52.3952704422441,32.05)) ;
#16455 = CARTESIAN_POINT('Ctrl Pts',(83.9875754901947,52.3601137381126,32.05)) ;
#16456 = CARTESIAN_POINT('Ctrl Pts',(83.9895070553043,52.3262319112097,32.05)) ;
#16457 = CARTESIAN_POINT('Ctrl Pts',(83.9936877046826,52.2925403287002,32.05)) ;
#16458 = CARTESIAN_POINT('Ctrl Pts',(84.0002271476368,52.2592666431595,32.05)) ;
#16459 = CARTESIAN_POINT('Ctrl Pts',(84.0055541232017,52.2321621770649,32.05)) ;
#16460 = CARTESIAN_POINT('Ctrl Pts',(84.0124471142095,52.2053351471932,32.05)) ;
#16461 = CARTESIAN_POINT('Ctrl Pts',(84.0209858286879,52.1789242467454,32.05)) ;
#16462 = CARTESIAN_POINT('Ctrl Pts',(84.4250317703929,52.9637142832168,26.3685084761921)) ;
#16463 = CARTESIAN_POINT('Ctrl Pts',(84.2056504531666,52.8563006564942,26.3895510373913)) ;
#16464 = CARTESIAN_POINT('Ctrl Pts',(83.8854653412497,52.4085896297169,26.4316361597899)) ;
#16465 = CARTESIAN_POINT('Ctrl Pts',(84.1861228684965,51.6345693759381,26.4947638433878)) ;
#16466 = CARTESIAN_POINT('Ctrl Pts',(84.998175822282,51.4645124050219,26.5578915269857)) ;
#16467 = CARTESIAN_POINT('Ctrl Pts',(85.5851072300976,52.0500826073856,26.6210192105835)) ;
#16468 = CARTESIAN_POINT('Ctrl Pts',(85.4162279933292,52.8622720429723,26.6841468941814)) ;
#16469 = CARTESIAN_POINT('Ctrl Pts',(84.6440981710049,53.1652507798167,26.7472745777793)) ;
#16470 = CARTESIAN_POINT('Ctrl Pts',(83.9678955818182,52.6849989840867,26.8104022613771)) ;
#16471 = CARTESIAN_POINT('Ctrl Pts',(83.9997130735727,51.8561601965047,26.873529944975)) ;
#16472 = CARTESIAN_POINT('Ctrl Pts',(84.710785203412,51.4291552942847,26.9366576285728)) ;
#16473 = CARTESIAN_POINT('Ctrl Pts',(85.4573524705639,51.7905235055957,26.9997853121707)) ;
#16474 = CARTESIAN_POINT('Ctrl Pts',(85.5635501520105,52.6131307432408,27.0629129957686)) ;
#16475 = CARTESIAN_POINT('Ctrl Pts',(84.933231811866,53.1522552393336,27.1260406793665)) ;
#16476 = CARTESIAN_POINT('Ctrl Pts',(84.1370327822058,52.9198264637372,27.1891683629643)) ;
#16477 = CARTESIAN_POINT('Ctrl Pts',(83.8957582643692,52.1262624336389,27.2522960465622)) ;
#16478 = CARTESIAN_POINT('Ctrl Pts',(84.4278368710099,51.4899849375734,27.31542373016)) ;
#16479 = CARTESIAN_POINT('Ctrl Pts',(85.2515726447776,51.5870214121571,27.3785514137579)) ;
#16480 = CARTESIAN_POINT('Ctrl Pts',(85.6212301121436,52.3295240675631,27.4416790973558)) ;
#16481 = CARTESIAN_POINT('Ctrl Pts',(85.2021548839321,53.0452982747,27.5048067809536)) ;
#16482 = CARTESIAN_POINT('Ctrl Pts',(84.3737396709075,53.0863470831135,27.5679344645515)) ;
#16483 = CARTESIAN_POINT('Ctrl Pts',(83.885956406241,52.4155085999048,27.6310621481494)) ;
#16484 = CARTESIAN_POINT('Ctrl Pts',(84.1803997961088,51.6400991179717,27.6941898317473)) ;
#16485 = CARTESIAN_POINT('Ctrl Pts',(84.9905075141293,51.4621040018937,27.7573175153451)) ;
#16486 = CARTESIAN_POINT('Ctrl Pts',(85.5828815572153,52.042663878742,27.820445198943)) ;
#16487 = CARTESIAN_POINT('Ctrl Pts',(85.4212402278205,52.8561925242217,27.8835728825408)) ;
#16488 = CARTESIAN_POINT('Ctrl Pts',(84.6519189159883,53.1661949368354,27.9467005661387)) ;
#16489 = CARTESIAN_POINT('Ctrl Pts',(83.9713913160093,52.6920230666678,28.0098282497366)) ;
#16490 = CARTESIAN_POINT('Ctrl Pts',(83.9957453544512,51.8629490907966,28.0729559333345)) ;
#16491 = CARTESIAN_POINT('Ctrl Pts',(84.7029330951489,51.4295413427059,28.1360836169323)) ;
#16492 = CARTESIAN_POINT('Ctrl Pts',(85.4527309398621,51.7841678628247,28.1992113005302)) ;
#16493 = CARTESIAN_POINT('Ctrl Pts',(85.5663399692938,52.6057819846142,28.2623389841281)) ;
#16494 = CARTESIAN_POINT('Ctrl Pts',(84.9409088790051,53.1505688493595,28.3254666677259)) ;
#16495 = CARTESIAN_POINT('Ctrl Pts',(84.1426462159603,52.9253278728757,28.3885943513238)) ;
#16496 = CARTESIAN_POINT('Ctrl Pts',(83.8942265474451,52.1339717931037,28.4517220349216)) ;
#16497 = CARTESIAN_POINT('Ctrl Pts',(84.4205464955366,51.4929225836516,28.5148497185195)) ;
#16498 = CARTESIAN_POINT('Ctrl Pts',(85.2451237463938,51.5825280191257,28.5779774021174)) ;
#16499 = CARTESIAN_POINT('Ctrl Pts',(85.6214608931572,52.3216674705582,28.6411050857152)) ;
#16500 = CARTESIAN_POINT('Ctrl Pts',(85.2088564383358,53.0411911606195,28.7042327693131)) ;
#16501 = CARTESIAN_POINT('Ctrl Pts',(84.3808450086281,53.08970764206,28.767360452911)) ;
#16502 = CARTESIAN_POINT('Ctrl Pts',(83.8870330047499,52.4232944957884,28.8304881365088)) ;
#16503 = CARTESIAN_POINT('Ctrl Pts',(84.1744729981709,51.6452617028549,28.8936158201067)) ;
#16504 = CARTESIAN_POINT('Ctrl Pts',(84.9829429060078,51.4599695421454,28.9567435037046)) ;
#16505 = CARTESIAN_POINT('Ctrl Pts',(85.5805274479185,52.0351647194261,29.0198711873024)) ;
#16506 = CARTESIAN_POINT('Ctrl Pts',(85.4262278145717,52.8501177241122,29.0829988709003)) ;
#16507 = CARTESIAN_POINT('Ctrl Pts',(84.6597328902445,53.1670440683605,29.1461265544982)) ;
#16508 = CARTESIAN_POINT('Ctrl Pts',(83.9749576147278,52.6990274033377,29.209254238096)) ;
#16509 = CARTESIAN_POINT('Ctrl Pts',(83.9918353744007,51.8697675418188,29.2723819216939)) ;
#16510 = CARTESIAN_POINT('Ctrl Pts',(84.6950865774281,51.4300011013776,29.3355096052917)) ;
#16511 = CARTESIAN_POINT('Ctrl Pts',(85.4480514094807,51.7778527053553,29.3986372888896)) ;
#16512 = CARTESIAN_POINT('Ctrl Pts',(85.5690638483639,52.5984090814401,29.4617649724875)) ;
#16513 = CARTESIAN_POINT('Ctrl Pts',(84.9485702146255,53.148812957869,29.5248926560853)) ;
#16514 = CARTESIAN_POINT('Ctrl Pts',(84.1483091301802,52.9307786178669,29.5880203396833)) ;
#16515 = CARTESIAN_POINT('Ctrl Pts',(83.8927643516779,52.1416945647534,29.6511480232811)) ;
#16516 = CARTESIAN_POINT('Ctrl Pts',(84.4132829291257,51.4959258854032,29.714275706879)) ;
#16517 = CARTESIAN_POINT('Ctrl Pts',(85.2386345831491,51.5780929341436,29.7774033904768)) ;
#16518 = CARTESIAN_POINT('Ctrl Pts',(85.6216208325441,52.3138091222706,29.8405310740747)) ;
#16519 = CARTESIAN_POINT('Ctrl Pts',(85.2155206857491,53.0370237843669,29.9036587576725)) ;
#16520 = CARTESIAN_POINT('Ctrl Pts',(84.3879803592861,53.0930040020832,29.9667864412704)) ;
#16521 = CARTESIAN_POINT('Ctrl Pts',(83.8881797597493,52.4310703668902,30.0299141248683)) ;
#16522 = CARTESIAN_POINT('Ctrl Pts',(84.1685929896107,51.6504775170526,30.0930418084662)) ;
#16523 = CARTESIAN_POINT('Ctrl Pts',(84.975359359988,51.4579033746375,30.156169492064)) ;
#16524 = CARTESIAN_POINT('Ctrl Pts',(85.5781058187447,52.0276870907513,30.2192971756619)) ;
#16525 = CARTESIAN_POINT('Ctrl Pts',(85.4311604255217,52.8439982006345,30.2824248592598)) ;
#16526 = CARTESIAN_POINT('Ctrl Pts',(84.6675542030255,53.1678227112312,30.3455525428576)) ;
#16527 = CARTESIAN_POINT('Ctrl Pts',(83.9785869226004,52.7059993000024,30.4086802264556)) ;
#16528 = CARTESIAN_POINT('Ctrl Pts',(83.9879870313722,51.8766209697171,30.4718079100533)) ;
#16529 = CARTESIAN_POINT('Ctrl Pts',(84.6872445240728,51.4305315890238,30.5349355936513)) ;
#16530 = CARTESIAN_POINT('Ctrl Pts',(85.4433151290645,51.7715799971008,30.5980632772491)) ;
#16531 = CARTESIAN_POINT('Ctrl Pts',(85.5717211395724,52.5910119186134,30.661190960847)) ;
#16532 = CARTESIAN_POINT('Ctrl Pts',(84.9562154066652,53.1469880592007,30.7243186444448)) ;
#16533 = CARTESIAN_POINT('Ctrl Pts',(84.1540209610485,52.9361780833212,30.7874463280427)) ;
#16534 = CARTESIAN_POINT('Ctrl Pts',(83.8913718460322,52.1494302036142,30.8505740116406)) ;
#16535 = CARTESIAN_POINT('Ctrl Pts',(84.406046739384,51.4989945619123,30.9137016952384)) ;
#16536 = CARTESIAN_POINT('Ctrl Pts',(85.2321056902744,51.5737165276034,30.9768293788363)) ;
#16537 = CARTESIAN_POINT('Ctrl Pts',(85.6217099208433,52.3059496735259,31.0399570624342)) ;
#16538 = CARTESIAN_POINT('Ctrl Pts',(85.2221470677742,53.0327964447449,31.103084746032)) ;
#16539 = CARTESIAN_POINT('Ctrl Pts',(84.3951451811447,53.0962359841114,31.1662124296299)) ;
#16540 = CARTESIAN_POINT('Ctrl Pts',(83.8893964978933,52.438835396788,31.2293401132277)) ;
#16541 = CARTESIAN_POINT('Ctrl Pts',(84.1627604121769,51.6557465123538,31.2924677968256)) ;
#16542 = CARTESIAN_POINT('Ctrl Pts',(84.9677571597911,51.4559049037231,31.3555954804235)) ;
#16543 = CARTESIAN_POINT('Ctrl Pts',(85.5756175422327,52.0202331507826,31.4187231640214)) ;
#16544 = CARTESIAN_POINT('Ctrl Pts',(85.4360362883285,52.8378313051878,31.4818508476192)) ;
#16545 = CARTESIAN_POINT('Ctrl Pts',(84.6753850015265,53.1685371869628,31.5449785312171)) ;
#16546 = CARTESIAN_POINT('Ctrl Pts',(83.9822732966132,52.7129252324505,31.608106214815)) ;
#16547 = CARTESIAN_POINT('Ctrl Pts',(83.9842121002569,51.883535113167,31.6712338984128)) ;
#16548 = CARTESIAN_POINT('Ctrl Pts',(84.6793843110363,51.4310793972544,31.7343615820107)) ;
#16549 = CARTESIAN_POINT('Ctrl Pts',(85.4385697001617,51.7654585545426,31.7974892656085)) ;
#16550 = CARTESIAN_POINT('Ctrl Pts',(85.5742157004875,52.583371203896,31.8606169492065)) ;
#16551 = CARTESIAN_POINT('Ctrl Pts',(84.9640410903861,53.1455422795452,31.9237446328042)) ;
#16552 = CARTESIAN_POINT('Ctrl Pts',(84.1593673264954,52.9405973219202,31.9868723164022)) ;
#16553 = CARTESIAN_POINT('Ctrl Pts',(83.9809659603427,52.4198895133115,32.0289574388007)) ;
#16554 = CARTESIAN_POINT('Ctrl Pts',(84.0209858286879,52.1789242467453,32.05)) ;
#16555 = CARTESIAN_POINT('Ctrl Pts',(84.3916481374235,53.031896930038,26.412338984128)) ;
#16556 = CARTESIAN_POINT('Ctrl Pts',(84.149730015958,52.9134488182067,26.4333815453273)) ;
#16557 = CARTESIAN_POINT('Ctrl Pts',(83.7966526355526,52.4197449243348,26.4754666677259)) ;
#16558 = CARTESIAN_POINT('Ctrl Pts',(84.1281963837424,51.5662104112876,26.5385943513238)) ;
#16559 = CARTESIAN_POINT('Ctrl Pts',(85.0236706547243,51.3786836726104,26.6017220349216)) ;
#16560 = CARTESIAN_POINT('Ctrl Pts',(85.6708968880384,52.0244088653162,26.6648497185195)) ;
#16561 = CARTESIAN_POINT('Ctrl Pts',(85.4846688708576,52.9200336387264,26.7279774021174)) ;
#16562 = CARTESIAN_POINT('Ctrl Pts',(84.6332189912334,53.2541370518524,26.7911050857152)) ;
#16563 = CARTESIAN_POINT('Ctrl Pts',(83.8875508451285,52.7245495112071,26.8542327693131)) ;
#16564 = CARTESIAN_POINT('Ctrl Pts',(83.9226369132237,51.8105650159697,26.917360452911)) ;
#16565 = CARTESIAN_POINT('Ctrl Pts',(84.7067567099872,51.3396943643224,26.9804881365088)) ;
#16566 = CARTESIAN_POINT('Ctrl Pts',(85.5300180209343,51.7381855391541,27.0436158201067)) ;
#16567 = CARTESIAN_POINT('Ctrl Pts',(85.647125274753,52.6452983241038,27.1067435037046)) ;
#16568 = CARTESIAN_POINT('Ctrl Pts',(84.9520550167161,53.2398064936223,27.1698711873024)) ;
#16569 = CARTESIAN_POINT('Ctrl Pts',(84.0740633262505,52.9835005625718,27.2329988709003)) ;
#16570 = CARTESIAN_POINT('Ctrl Pts',(83.8080029394754,52.1084145623087,27.2961265544982)) ;
#16571 = CARTESIAN_POINT('Ctrl Pts',(84.3947414029776,51.4067729707409,27.359254238096)) ;
#16572 = CARTESIAN_POINT('Ctrl Pts',(85.3030986573388,51.5137778968747,27.4223819216939)) ;
#16573 = CARTESIAN_POINT('Ctrl Pts',(85.7107306344894,52.3325570429296,27.4855096052918)) ;
#16574 = CARTESIAN_POINT('Ctrl Pts',(85.2486042636415,53.12186195628,27.5486372888896)) ;
#16575 = CARTESIAN_POINT('Ctrl Pts',(84.3350868563152,53.1671276641595,27.6117649724875)) ;
#16576 = CARTESIAN_POINT('Ctrl Pts',(83.7971941471168,52.4273746728089,27.6748926560853)) ;
#16577 = CARTESIAN_POINT('Ctrl Pts',(84.1218853863496,51.5723082177092,27.7380203396832)) ;
#16578 = CARTESIAN_POINT('Ctrl Pts',(85.015214589611,51.3760278568469,27.8011480232811)) ;
#16579 = CARTESIAN_POINT('Ctrl Pts',(85.6684425742004,52.0162280187436,27.8642757068789)) ;
#16580 = CARTESIAN_POINT('Ctrl Pts',(85.4901960067496,52.9133295776232,27.9274033904768)) ;
#16581 = CARTESIAN_POINT('Ctrl Pts',(84.6418431528474,53.2551782010954,27.9905310740747)) ;
#16582 = CARTESIAN_POINT('Ctrl Pts',(83.891405692293,52.7322951701561,28.0536587576726)) ;
#16583 = CARTESIAN_POINT('Ctrl Pts',(83.91826159463,51.8180513259923,28.1167864412704)) ;
#16584 = CARTESIAN_POINT('Ctrl Pts',(84.6980979631779,51.3401200710782,28.1799141248683)) ;
#16585 = CARTESIAN_POINT('Ctrl Pts',(85.5249217254073,51.7311769881103,28.2430418084661)) ;
#16586 = CARTESIAN_POINT('Ctrl Pts',(85.6502016869332,52.637194635492,28.306169492064)) ;
#16587 = CARTESIAN_POINT('Ctrl Pts',(84.9605207406171,53.2379468626393,28.3692971756619)) ;
#16588 = CARTESIAN_POINT('Ctrl Pts',(84.0802534219525,52.9895671254908,28.4324248592598)) ;
#16589 = CARTESIAN_POINT('Ctrl Pts',(83.8063138709369,52.116915895891,28.4955525428576)) ;
#16590 = CARTESIAN_POINT('Ctrl Pts',(84.3867020951568,51.4100123980073,28.5586802264555)) ;
#16591 = CARTESIAN_POINT('Ctrl Pts',(85.2959872706344,51.5088229024618,28.6218079100534)) ;
#16592 = CARTESIAN_POINT('Ctrl Pts',(85.7109851233857,52.3238933462549,28.6849355936512)) ;
#16593 = CARTESIAN_POINT('Ctrl Pts',(85.255994261444,53.1173329228348,28.7480632772491)) ;
#16594 = CARTESIAN_POINT('Ctrl Pts',(84.3429221176562,53.1708334496735,28.8111909608469)) ;
#16595 = CARTESIAN_POINT('Ctrl Pts',(83.7983813434201,52.435960405313,28.8743186444449)) ;
#16596 = CARTESIAN_POINT('Ctrl Pts',(84.1153497349023,51.5780011493255,28.9374463280427)) ;
#16597 = CARTESIAN_POINT('Ctrl Pts',(85.0068728775201,51.3736741263689,29.0005740116406)) ;
#16598 = CARTESIAN_POINT('Ctrl Pts',(85.6658466298146,52.0079584789432,29.0637016952384)) ;
#16599 = CARTESIAN_POINT('Ctrl Pts',(85.495695962866,52.9066307199022,29.1268293788363)) ;
#16600 = CARTESIAN_POINT('Ctrl Pts',(84.6504598481846,53.256114562979,29.1899570624342)) ;
#16601 = CARTESIAN_POINT('Ctrl Pts',(83.8953383530021,52.740019054718,29.253084746032)) ;
#16602 = CARTESIAN_POINT('Ctrl Pts',(83.9139499465792,51.8255702290761,29.3162124296299)) ;
#16603 = CARTESIAN_POINT('Ctrl Pts',(84.6894453812211,51.3406270602584,29.3793401132277)) ;
#16604 = CARTESIAN_POINT('Ctrl Pts',(85.5197614719567,51.7242130813791,29.4424677968257)) ;
#16605 = CARTESIAN_POINT('Ctrl Pts',(85.6532053871393,52.6290643219895,29.5055954804234)) ;
#16606 = CARTESIAN_POINT('Ctrl Pts',(84.9689691169173,53.2360105903249,29.5687231640214)) ;
#16607 = CARTESIAN_POINT('Ctrl Pts',(84.0864980811943,52.9955778195896,29.6318508476192)) ;
#16608 = CARTESIAN_POINT('Ctrl Pts',(83.8047014653877,52.1254320194772,29.6949785312171)) ;
#16609 = CARTESIAN_POINT('Ctrl Pts',(84.3786923504646,51.4133242256831,29.7581062148149)) ;
#16610 = CARTESIAN_POINT('Ctrl Pts',(85.2888314827036,51.5039322060206,29.8212338984128)) ;
#16611 = CARTESIAN_POINT('Ctrl Pts',(85.7111614931719,52.3152277183902,29.8843615820107)) ;
#16612 = CARTESIAN_POINT('Ctrl Pts',(85.2633431197498,53.1127374365499,29.9474892656085)) ;
#16613 = CARTESIAN_POINT('Ctrl Pts',(84.3507904751306,53.1744684411786,30.0106169492064)) ;
#16614 = CARTESIAN_POINT('Ctrl Pts',(83.799645903314,52.4445350832003,30.0737446328043)) ;
#16615 = CARTESIAN_POINT('Ctrl Pts',(84.1088656794546,51.5837527784458,30.1368723164022)) ;
#16616 = CARTESIAN_POINT('Ctrl Pts',(84.9985102820616,51.371395703719,30.2)) ;
#16617 = CARTESIAN_POINT('Ctrl Pts',(85.6631762293081,51.9997126816031,30.2631276835979)) ;
#16618 = CARTESIAN_POINT('Ctrl Pts',(85.5011352955771,52.8998825444299,30.3262553671958)) ;
#16619 = CARTESIAN_POINT('Ctrl Pts',(84.6590846359253,53.2569731949853,30.3893830507936)) ;
#16620 = CARTESIAN_POINT('Ctrl Pts',(83.8993404957274,52.7477071667482,30.4525107343915)) ;
#16621 = CARTESIAN_POINT('Ctrl Pts',(83.9097062674547,51.8331277021723,30.5156384179893)) ;
#16622 = CARTESIAN_POINT('Ctrl Pts',(84.6807977222494,51.3412120443238,30.5787661015873)) ;
#16623 = CARTESIAN_POINT('Ctrl Pts',(85.5145386386019,51.7172959846245,30.641893785185)) ;
#16624 = CARTESIAN_POINT('Ctrl Pts',(85.656135658985,52.6209072566667,30.705021468783)) ;
#16625 = CARTESIAN_POINT('Ctrl Pts',(84.9773996912245,53.2339982218002,30.7681491523808)) ;
#16626 = CARTESIAN_POINT('Ctrl Pts',(84.0927966822388,53.0015319662604,30.8312768359787)) ;
#16627 = CARTESIAN_POINT('Ctrl Pts',(83.8031659091507,52.1339623321091,30.8944045195766)) ;
#16628 = CARTESIAN_POINT('Ctrl Pts',(84.370712794817,51.4167081439941,30.9575322031743)) ;
#16629 = CARTESIAN_POINT('Ctrl Pts',(85.281631883761,51.499106215994,31.0206598867723)) ;
#16630 = CARTESIAN_POINT('Ctrl Pts',(85.7112597334154,52.3065608770196,31.0837875703701)) ;
#16631 = CARTESIAN_POINT('Ctrl Pts',(85.2706502227969,53.1080758269238,31.146915253968)) ;
#16632 = CARTESIAN_POINT('Ctrl Pts',(84.3586913313503,53.1780324412071,31.2100429375659)) ;
#16633 = CARTESIAN_POINT('Ctrl Pts',(83.800987635645,52.4530978061784,31.2731706211637)) ;
#16634 = CARTESIAN_POINT('Ctrl Pts',(84.1024339276812,51.5895630519065,31.3362983047616)) ;
#16635 = CARTESIAN_POINT('Ctrl Pts',(84.9901271161026,51.3691919320601,31.3994259883595)) ;
#16636 = CARTESIAN_POINT('Ctrl Pts',(85.660432334855,51.9914930064843,31.4625536719573)) ;
#16637 = CARTESIAN_POINT('Ctrl Pts',(85.5065120504696,52.8930821305178,31.5256813555552)) ;
#16638 = CARTESIAN_POINT('Ctrl Pts',(84.6677198838439,53.2577610680321,31.588809039153)) ;
#16639 = CARTESIAN_POINT('Ctrl Pts',(83.9034055669352,52.7553445927079,31.6519367227509)) ;
#16640 = CARTESIAN_POINT('Ctrl Pts',(83.9055435417695,51.8407521280628,31.7150644063488)) ;
#16641 = CARTESIAN_POINT('Ctrl Pts',(84.6721300380722,51.3418161282985,31.7781920899467)) ;
#16642 = CARTESIAN_POINT('Ctrl Pts',(85.5093057169464,51.7105456929264,31.8413197735445)) ;
#16643 = CARTESIAN_POINT('Ctrl Pts',(85.6588864834312,52.6124816196323,31.9044474571424)) ;
#16644 = CARTESIAN_POINT('Ctrl Pts',(84.9860292989271,53.2324039187721,31.9675751407402)) ;
#16645 = CARTESIAN_POINT('Ctrl Pts',(84.0986922739962,53.0064051884369,32.0307028243381)) ;
#16646 = CARTESIAN_POINT('Ctrl Pts',(83.9019639294307,52.4322056326875,32.0727879467367)) ;
#16647 = CARTESIAN_POINT('Ctrl Pts',(83.9460949953472,52.1664862662295,32.093830507936)) ;
#16648 = CARTESIAN_POINT('Ctrl Pts',(84.3582645044542,53.1000795768593,26.456169492064)) ;
#16649 = CARTESIAN_POINT('Ctrl Pts',(84.0938095787495,52.9705969799192,26.4772120532633)) ;
#16650 = CARTESIAN_POINT('Ctrl Pts',(83.7078399298555,52.4309002189528,26.5192971756619)) ;
#16651 = CARTESIAN_POINT('Ctrl Pts',(84.0702698989883,51.4978514466372,26.5824248592598)) ;
#16652 = CARTESIAN_POINT('Ctrl Pts',(85.0491654871666,51.292854940199,26.6455525428576)) ;
#16653 = CARTESIAN_POINT('Ctrl Pts',(85.7566865459792,51.9987351232468,26.7086802264555)) ;
#16654 = CARTESIAN_POINT('Ctrl Pts',(85.553109748386,52.9777952344805,26.7718079100534)) ;
#16655 = CARTESIAN_POINT('Ctrl Pts',(84.6223398114619,53.3430233238882,26.8349355936512)) ;
#16656 = CARTESIAN_POINT('Ctrl Pts',(83.8072061084389,52.7641000383273,26.8980632772491)) ;
#16657 = CARTESIAN_POINT('Ctrl Pts',(83.8455607528747,51.7649698354348,26.961190960847)) ;
#16658 = CARTESIAN_POINT('Ctrl Pts',(84.7027282165623,51.2502334343599,27.0243186444448)) ;
#16659 = CARTESIAN_POINT('Ctrl Pts',(85.6026835713044,51.6858475727128,27.0874463280427)) ;
#16660 = CARTESIAN_POINT('Ctrl Pts',(85.7307003974957,52.6774659049666,27.1505740116405)) ;
#16661 = CARTESIAN_POINT('Ctrl Pts',(84.9708782215659,53.3273577479112,27.2137016952384)) ;
#16662 = CARTESIAN_POINT('Ctrl Pts',(84.0110938702955,53.0471746614063,27.2768293788363)) ;
#16663 = CARTESIAN_POINT('Ctrl Pts',(83.7202476145812,52.0905666909787,27.3399570624342)) ;
#16664 = CARTESIAN_POINT('Ctrl Pts',(84.3616459349454,51.3235610039085,27.403084746032)) ;
#16665 = CARTESIAN_POINT('Ctrl Pts',(85.3546246698999,51.4405343815921,27.4662124296299)) ;
#16666 = CARTESIAN_POINT('Ctrl Pts',(85.8002311568352,52.335590018296,27.5293401132277)) ;
#16667 = CARTESIAN_POINT('Ctrl Pts',(85.295053643351,53.1984256378601,27.5924677968256)) ;
#16668 = CARTESIAN_POINT('Ctrl Pts',(84.2964340417231,53.2479082452055,27.6555954804235)) ;
#16669 = CARTESIAN_POINT('Ctrl Pts',(83.7084318879924,52.439240745713,27.7187231640213)) ;
#16670 = CARTESIAN_POINT('Ctrl Pts',(84.0633709765903,51.5045173174467,27.7818508476192)) ;
#16671 = CARTESIAN_POINT('Ctrl Pts',(85.0399216650928,51.2899517118001,27.8449785312171)) ;
#16672 = CARTESIAN_POINT('Ctrl Pts',(85.7540035911854,51.9897921587451,27.908106214815)) ;
#16673 = CARTESIAN_POINT('Ctrl Pts',(85.5591517856788,52.9704666310249,27.9712338984128)) ;
#16674 = CARTESIAN_POINT('Ctrl Pts',(84.6317673897063,53.3441614653553,28.0343615820107)) ;
#16675 = CARTESIAN_POINT('Ctrl Pts',(83.8114200685767,52.7725672736444,28.0974892656085)) ;
#16676 = CARTESIAN_POINT('Ctrl Pts',(83.8407778348087,51.773153561188,28.1606169492064)) ;
#16677 = CARTESIAN_POINT('Ctrl Pts',(84.6932628312068,51.2506987994505,28.2237446328043)) ;
#16678 = CARTESIAN_POINT('Ctrl Pts',(85.5971125109525,51.678186113396,28.2868723164021)) ;
#16679 = CARTESIAN_POINT('Ctrl Pts',(85.7340634045725,52.6686072863696,28.35)) ;
#16680 = CARTESIAN_POINT('Ctrl Pts',(84.980132602229,53.3253248759193,28.4131276835978)) ;
#16681 = CARTESIAN_POINT('Ctrl Pts',(84.0178606279449,53.0538063781057,28.4762553671958)) ;
#16682 = CARTESIAN_POINT('Ctrl Pts',(83.7184011944283,52.0998599986783,28.5393830507936)) ;
#16683 = CARTESIAN_POINT('Ctrl Pts',(84.3528576947773,51.3271022123631,28.6025107343915)) ;
#16684 = CARTESIAN_POINT('Ctrl Pts',(85.3468507948749,51.4351177857977,28.6656384179893)) ;
#16685 = CARTESIAN_POINT('Ctrl Pts',(85.8005093536141,52.3261192219517,28.7287661015872)) ;
#16686 = CARTESIAN_POINT('Ctrl Pts',(85.3031320845523,53.1934746850499,28.7918937851851)) ;
#16687 = CARTESIAN_POINT('Ctrl Pts',(84.3049992266842,53.2519592572871,28.8550214687829)) ;
#16688 = CARTESIAN_POINT('Ctrl Pts',(83.7097296820902,52.4486263148374,28.9181491523808)) ;
#16689 = CARTESIAN_POINT('Ctrl Pts',(84.0562264716337,51.5107405957961,28.9812768359787)) ;
#16690 = CARTESIAN_POINT('Ctrl Pts',(85.0308028490327,51.2873787105924,29.0444045195765)) ;
#16691 = CARTESIAN_POINT('Ctrl Pts',(85.7511658117106,51.9807522384602,29.1075322031744)) ;
#16692 = CARTESIAN_POINT('Ctrl Pts',(85.5651641111605,52.9631437156923,29.1706598867723)) ;
#16693 = CARTESIAN_POINT('Ctrl Pts',(84.6411868061246,53.3451850575975,29.2337875703701)) ;
#16694 = CARTESIAN_POINT('Ctrl Pts',(83.8157190912767,52.7810107060983,29.296915253968)) ;
#16695 = CARTESIAN_POINT('Ctrl Pts',(83.8360645187576,51.7813729163333,29.3600429375658)) ;
#16696 = CARTESIAN_POINT('Ctrl Pts',(84.6838041850143,51.2512530191392,29.4231706211637)) ;
#16697 = CARTESIAN_POINT('Ctrl Pts',(85.5914715344326,51.6705734574028,29.4862983047616)) ;
#16698 = CARTESIAN_POINT('Ctrl Pts',(85.7373469259147,52.6597195625389,29.5494259883594)) ;
#16699 = CARTESIAN_POINT('Ctrl Pts',(84.9893680192092,53.3232082227807,29.6125536719573)) ;
#16700 = CARTESIAN_POINT('Ctrl Pts',(84.0246870322085,53.0603770213123,29.6756813555552)) ;
#16701 = CARTESIAN_POINT('Ctrl Pts',(83.7166385790976,52.109169474201,29.7388090391531)) ;
#16702 = CARTESIAN_POINT('Ctrl Pts',(84.3441017718036,51.330722565963,29.8019367227509)) ;
#16703 = CARTESIAN_POINT('Ctrl Pts',(85.339028382258,51.4297714778975,29.8650644063488)) ;
#16704 = CARTESIAN_POINT('Ctrl Pts',(85.8007021537997,52.3166463145098,29.9281920899466)) ;
#16705 = CARTESIAN_POINT('Ctrl Pts',(85.3111655537503,53.1884510887328,29.9913197735445)) ;
#16706 = CARTESIAN_POINT('Ctrl Pts',(84.3136005909752,53.2559328802739,30.0544474571424)) ;
#16707 = CARTESIAN_POINT('Ctrl Pts',(83.7111120468786,52.4579997995102,30.1175751407403)) ;
#16708 = CARTESIAN_POINT('Ctrl Pts',(84.0491383692985,51.5170280398391,30.1807028243381)) ;
#16709 = CARTESIAN_POINT('Ctrl Pts',(85.0216612041352,51.2848880328004,30.243830507936)) ;
#16710 = CARTESIAN_POINT('Ctrl Pts',(85.7482466398716,51.971738272455,30.3069581915338)) ;
#16711 = CARTESIAN_POINT('Ctrl Pts',(85.5711101656323,52.9557668882253,30.3700858751317)) ;
#16712 = CARTESIAN_POINT('Ctrl Pts',(84.6506150688253,53.3461236787394,30.4332135587296)) ;
#16713 = CARTESIAN_POINT('Ctrl Pts',(83.8200940688542,52.7894150334941,30.4963412423275)) ;
#16714 = CARTESIAN_POINT('Ctrl Pts',(83.8314255035372,51.7896344346275,30.5594689259253)) ;
#16715 = CARTESIAN_POINT('Ctrl Pts',(84.6743509204261,51.2518924996238,30.6225966095232)) ;
#16716 = CARTESIAN_POINT('Ctrl Pts',(85.5857621481392,51.663011972148,30.685724293121)) ;
#16717 = CARTESIAN_POINT('Ctrl Pts',(85.7405501783976,52.65080259472,30.7488519767189)) ;
#16718 = CARTESIAN_POINT('Ctrl Pts',(84.9985839757837,53.3210083843996,30.8119796603168)) ;
#16719 = CARTESIAN_POINT('Ctrl Pts',(84.0315724034291,53.0668858491997,30.8751073439147)) ;
#16720 = CARTESIAN_POINT('Ctrl Pts',(83.7149599722692,52.118494460604,30.9382350275124)) ;
#16721 = CARTESIAN_POINT('Ctrl Pts',(84.3353788502498,51.334421726076,31.0013627111105)) ;
#16722 = CARTESIAN_POINT('Ctrl Pts',(85.3311580772478,51.4244959043844,31.0644903947082)) ;
#16723 = CARTESIAN_POINT('Ctrl Pts',(85.8008095459872,52.3071720805132,31.1276180783062)) ;
#16724 = CARTESIAN_POINT('Ctrl Pts',(85.3191533778198,53.1833552091027,31.190745761904)) ;
#16725 = CARTESIAN_POINT('Ctrl Pts',(84.3222374815559,53.2598288983029,31.2538734455018)) ;
#16726 = CARTESIAN_POINT('Ctrl Pts',(83.7125787733965,52.4673602155687,31.3170011290997)) ;
#16727 = CARTESIAN_POINT('Ctrl Pts',(84.0421074431857,51.5233795914594,31.3801288126976)) ;
#16728 = CARTESIAN_POINT('Ctrl Pts',(85.0124970724141,51.282478960397,31.4432564962955)) ;
#16729 = CARTESIAN_POINT('Ctrl Pts',(85.7452471274772,51.962752862186,31.5063841798933)) ;
#16730 = CARTESIAN_POINT('Ctrl Pts',(85.5769878126107,52.9483329558477,31.5695118634912)) ;
#16731 = CARTESIAN_POINT('Ctrl Pts',(84.6600547661612,53.3469849491015,31.632639547089)) ;
#16732 = CARTESIAN_POINT('Ctrl Pts',(83.8245378372572,52.7977639529653,31.6957672306869)) ;
#16733 = CARTESIAN_POINT('Ctrl Pts',(83.8268749832821,51.7979691429585,31.7588949142848)) ;
#16734 = CARTESIAN_POINT('Ctrl Pts',(84.6648757651081,51.2525528593426,31.8220225978826)) ;
#16735 = CARTESIAN_POINT('Ctrl Pts',(85.5800417337311,51.6556328313103,31.8851502814805)) ;
#16736 = CARTESIAN_POINT('Ctrl Pts',(85.7435572663748,52.6415920353685,31.9482779650784)) ;
#16737 = CARTESIAN_POINT('Ctrl Pts',(85.0080175074681,53.3192655579993,32.0114056486762)) ;
#16738 = CARTESIAN_POINT('Ctrl Pts',(84.0380172214971,53.0722130549535,32.0745333322741)) ;
#16739 = CARTESIAN_POINT('Ctrl Pts',(83.8229618985187,52.4445217520636,32.1166184546727)) ;
#16740 = CARTESIAN_POINT('Ctrl Pts',(83.8712041620066,52.1540482857136,32.137661015872)) ;
#16741 = CARTESIAN_POINT('Ctrl Pts',(84.3248808714849,53.1682622236805,26.5)) ;
#16742 = CARTESIAN_POINT('Ctrl Pts',(84.037889141541,53.0277451416317,26.5210425611993)) ;
#16743 = CARTESIAN_POINT('Ctrl Pts',(83.6190272241585,52.4420555135708,26.5631276835978)) ;
#16744 = CARTESIAN_POINT('Ctrl Pts',(84.0123434142341,51.4294924819867,26.6262553671958)) ;
#16745 = CARTESIAN_POINT('Ctrl Pts',(85.074660319609,51.2070262077874,26.6893830507936)) ;
#16746 = CARTESIAN_POINT('Ctrl Pts',(85.8424762039199,51.9730613811773,26.7525107343915)) ;
#16747 = CARTESIAN_POINT('Ctrl Pts',(85.6215506259147,53.0355568302346,26.8156384179893)) ;
#16748 = CARTESIAN_POINT('Ctrl Pts',(84.6114606316903,53.4319095959239,26.8787661015872)) ;
#16749 = CARTESIAN_POINT('Ctrl Pts',(83.7268613717493,52.8036505654477,26.941893785185)) ;
#16750 = CARTESIAN_POINT('Ctrl Pts',(83.7684845925257,51.7193746548998,27.0050214687829)) ;
#16751 = CARTESIAN_POINT('Ctrl Pts',(84.6986997231375,51.1607725043976,27.0681491523808)) ;
#16752 = CARTESIAN_POINT('Ctrl Pts',(85.6753491216747,51.6335096062714,27.1312768359787)) ;
#16753 = CARTESIAN_POINT('Ctrl Pts',(85.8142755202384,52.7096334858295,27.1944045195765)) ;
#16754 = CARTESIAN_POINT('Ctrl Pts',(84.989701426416,53.4149090021999,27.2575322031744)) ;
#16755 = CARTESIAN_POINT('Ctrl Pts',(83.9481244143403,53.1108487602408,27.3206598867722)) ;
#16756 = CARTESIAN_POINT('Ctrl Pts',(83.6324922896873,52.0727188196486,27.3837875703701)) ;
#16757 = CARTESIAN_POINT('Ctrl Pts',(84.3285504669132,51.240349037076,27.446915253968)) ;
#16758 = CARTESIAN_POINT('Ctrl Pts',(85.406150682461,51.3672908663097,27.5100429375659)) ;
#16759 = CARTESIAN_POINT('Ctrl Pts',(85.8897316791811,52.3386229936625,27.5731706211637)) ;
#16760 = CARTESIAN_POINT('Ctrl Pts',(85.3415030230601,53.2749893194401,27.6362983047616)) ;
#16761 = CARTESIAN_POINT('Ctrl Pts',(84.257781227131,53.3286888262516,27.6994259883595)) ;
#16762 = CARTESIAN_POINT('Ctrl Pts',(83.6196696288681,52.451106818617,27.7625536719573)) ;
#16763 = CARTESIAN_POINT('Ctrl Pts',(84.0048565668312,51.4367264171842,27.8256813555552)) ;
#16764 = CARTESIAN_POINT('Ctrl Pts',(85.0646287405743,51.2038755667533,27.8888090391531)) ;
#16765 = CARTESIAN_POINT('Ctrl Pts',(85.8395646081705,51.9633562987467,27.9519367227509)) ;
#16766 = CARTESIAN_POINT('Ctrl Pts',(85.628107564608,53.0276036844266,28.0150644063488)) ;
#16767 = CARTESIAN_POINT('Ctrl Pts',(84.6216916265653,53.4331447296151,28.0781920899466)) ;
#16768 = CARTESIAN_POINT('Ctrl Pts',(83.7314344448605,52.8128393771328,28.1413197735445)) ;
#16769 = CARTESIAN_POINT('Ctrl Pts',(83.7632940749875,51.7282557963837,28.2044474571424)) ;
#16770 = CARTESIAN_POINT('Ctrl Pts',(84.6884276992357,51.1612775278227,28.2675751407402)) ;
#16771 = CARTESIAN_POINT('Ctrl Pts',(85.6693032964976,51.6251952386817,28.3307028243381)) ;
#16772 = CARTESIAN_POINT('Ctrl Pts',(85.817925122212,52.7000199372473,28.393830507936)) ;
#16773 = CARTESIAN_POINT('Ctrl Pts',(84.9997444638408,53.4127028891992,28.4569581915338)) ;
#16774 = CARTESIAN_POINT('Ctrl Pts',(83.9554678339372,53.1180456307208,28.5200858751317)) ;
#16775 = CARTESIAN_POINT('Ctrl Pts',(83.6304885179198,52.0828041014656,28.5832135587296)) ;
#16776 = CARTESIAN_POINT('Ctrl Pts',(84.3190132943977,51.2441920267188,28.6463412423274)) ;
#16777 = CARTESIAN_POINT('Ctrl Pts',(85.3977143191155,51.3614126691337,28.7094689259253)) ;
#16778 = CARTESIAN_POINT('Ctrl Pts',(85.8900335838426,52.3283450976483,28.7725966095232)) ;
#16779 = CARTESIAN_POINT('Ctrl Pts',(85.3502699076606,53.2696164472651,28.835724293121)) ;
#16780 = CARTESIAN_POINT('Ctrl Pts',(84.2670763357121,53.3330850649006,28.8988519767189)) ;
#16781 = CARTESIAN_POINT('Ctrl Pts',(83.6210780207605,52.4612922243619,28.9619796603168)) ;
#16782 = CARTESIAN_POINT('Ctrl Pts',(83.997103208365,51.4434800422666,29.0251073439146)) ;
#16783 = CARTESIAN_POINT('Ctrl Pts',(85.0547328205452,51.201083294816,29.0882350275125)) ;
#16784 = CARTESIAN_POINT('Ctrl Pts',(85.8364849936065,51.9535459979772,29.1513627111104)) ;
#16785 = CARTESIAN_POINT('Ctrl Pts',(85.6346322594548,53.0196567114824,29.2144903947082)) ;
#16786 = CARTESIAN_POINT('Ctrl Pts',(84.6319137640648,53.4342555522159,29.2776180783061)) ;
#16787 = CARTESIAN_POINT('Ctrl Pts',(83.7360998295509,52.8220023574787,29.3407457619039)) ;
#16788 = CARTESIAN_POINT('Ctrl Pts',(83.7581790909362,51.7371756035905,29.4038734455019)) ;
#16789 = CARTESIAN_POINT('Ctrl Pts',(84.6781629888073,51.16187897802,29.4670011290997)) ;
#16790 = CARTESIAN_POINT('Ctrl Pts',(85.6631815969086,51.6169338334265,29.5301288126976)) ;
#16791 = CARTESIAN_POINT('Ctrl Pts',(85.82148846469,52.6903748030883,29.5932564962954)) ;
#16792 = CARTESIAN_POINT('Ctrl Pts',(85.009766921501,53.4104058552366,29.6563841798933)) ;
#16793 = CARTESIAN_POINT('Ctrl Pts',(83.9628759832229,53.125176223035,29.7195118634911)) ;
#16794 = CARTESIAN_POINT('Ctrl Pts',(83.6285756928073,52.0929069289247,29.782639547089)) ;
#16795 = CARTESIAN_POINT('Ctrl Pts',(84.3095111931425,51.248120906243,29.8457672306869)) ;
#16796 = CARTESIAN_POINT('Ctrl Pts',(85.3892252818123,51.3556107497744,29.9088949142848)) ;
#16797 = CARTESIAN_POINT('Ctrl Pts',(85.8902428144277,52.3180649106294,29.9720225978826)) ;
#16798 = CARTESIAN_POINT('Ctrl Pts',(85.3589879877509,53.2641647409157,30.0351502814805)) ;
#16799 = CARTESIAN_POINT('Ctrl Pts',(84.2764107068199,53.3373973193694,30.0982779650783)) ;
#16800 = CARTESIAN_POINT('Ctrl Pts',(83.6225781904432,52.4714645158203,30.1614056486763)) ;
#16801 = CARTESIAN_POINT('Ctrl Pts',(83.9894110591425,51.4503033012323,30.2245333322741)) ;
#16802 = CARTESIAN_POINT('Ctrl Pts',(85.0448121262088,51.198380361882,30.287661015872)) ;
#16803 = CARTESIAN_POINT('Ctrl Pts',(85.833317050435,51.9437638633069,30.3507886994698)) ;
#16804 = CARTESIAN_POINT('Ctrl Pts',(85.6410850356875,53.0116512320208,30.4139163830677)) ;
#16805 = CARTESIAN_POINT('Ctrl Pts',(84.6421455017252,53.4352741624935,30.4770440666656)) ;
#16806 = CARTESIAN_POINT('Ctrl Pts',(83.7408476419811,52.8311229002399,30.5401717502634)) ;
#16807 = CARTESIAN_POINT('Ctrl Pts',(83.7531447396198,51.7461411670827,30.6032994338613)) ;
#16808 = CARTESIAN_POINT('Ctrl Pts',(84.6679041186026,51.1625729549238,30.6664271174591)) ;
#16809 = CARTESIAN_POINT('Ctrl Pts',(85.6569856576766,51.6087279596716,30.729554801057)) ;
#16810 = CARTESIAN_POINT('Ctrl Pts',(85.8249646978101,52.6806979327732,30.7926824846549)) ;
#16811 = CARTESIAN_POINT('Ctrl Pts',(85.019768260343,53.4080185469991,30.8558101682527)) ;
#16812 = CARTESIAN_POINT('Ctrl Pts',(83.9703481246194,53.132239732139,30.9189378518507)) ;
#16813 = CARTESIAN_POINT('Ctrl Pts',(83.6267540353877,52.1030265890989,30.9820655354484)) ;
#16814 = CARTESIAN_POINT('Ctrl Pts',(84.3000449056827,51.2521353081579,31.0451932190464)) ;
#16815 = CARTESIAN_POINT('Ctrl Pts',(85.3806842707344,51.3498855927749,31.1083209026442)) ;
#16816 = CARTESIAN_POINT('Ctrl Pts',(85.8903593585592,52.3077832840069,31.1714485862421)) ;
#16817 = CARTESIAN_POINT('Ctrl Pts',(85.3676565328426,53.2586345912816,31.2345762698399)) ;
#16818 = CARTESIAN_POINT('Ctrl Pts',(84.2857836317614,53.3416253553987,31.2977039534379)) ;
#16819 = CARTESIAN_POINT('Ctrl Pts',(83.6241699111481,52.4816226249592,31.3608316370356)) ;
#16820 = CARTESIAN_POINT('Ctrl Pts',(83.9817809586901,51.4571961310121,31.4239593206336)) ;
#16821 = CARTESIAN_POINT('Ctrl Pts',(85.0348670287255,51.195765988734,31.4870870042314)) ;
#16822 = CARTESIAN_POINT('Ctrl Pts',(85.8300619200994,51.9340127178877,31.5502146878293)) ;
#16823 = CARTESIAN_POINT('Ctrl Pts',(85.6474635747518,53.0035837811777,31.6133423714272)) ;
#16824 = CARTESIAN_POINT('Ctrl Pts',(84.6523896484787,53.4362088301708,31.676470055025)) ;
#16825 = CARTESIAN_POINT('Ctrl Pts',(83.745670107579,52.8401833132227,31.7395977386229)) ;
#16826 = CARTESIAN_POINT('Ctrl Pts',(83.7482064247947,51.7551861578542,31.8027254222207)) ;
#16827 = CARTESIAN_POINT('Ctrl Pts',(84.657621492144,51.1632895903866,31.8658531058187)) ;
#16828 = CARTESIAN_POINT('Ctrl Pts',(85.6507777505159,51.6007199696942,31.9289807894165)) ;
#16829 = CARTESIAN_POINT('Ctrl Pts',(85.8282280493184,52.6707024511047,31.9921084730144)) ;
#16830 = CARTESIAN_POINT('Ctrl Pts',(85.0300057160091,53.4061271972263,32.0552361566122)) ;
#16831 = CARTESIAN_POINT('Ctrl Pts',(83.9773421689979,53.1380209214701,32.1183638402101)) ;
#16832 = CARTESIAN_POINT('Ctrl Pts',(83.7439598676067,52.4568378714396,32.1604489626087)) ;
#16833 = CARTESIAN_POINT('Ctrl Pts',(83.7963133286659,52.1416103051977,32.1814915238079)) ;
#16834 = CARTESIAN_POINT('Ctrl Pts',(83.7847716506988,52.3000190203057,31.7710140831103)) ;
#16835 = CARTESIAN_POINT('Ctrl Pts',(83.7847913222747,52.1388962198161,31.7815845294805)) ;
#16836 = CARTESIAN_POINT('Ctrl Pts',(83.8230018066232,51.977763740797,31.7921549758506)) ;
#16837 = CARTESIAN_POINT('Ctrl Pts',(83.8993528831503,51.837369589171,31.8027254222207)) ;
#16838 = CARTESIAN_POINT('Ctrl Pts',(84.0513447805778,51.5578873020316,31.82376798342)) ;
#16839 = CARTESIAN_POINT('Ctrl Pts',(84.3544831363609,51.3605884462091,31.8448105446193)) ;
#16840 = CARTESIAN_POINT('Ctrl Pts',(84.6715783573144,51.3348440815158,31.8658531058186)) ;
#16841 = CARTESIAN_POINT('Ctrl Pts',(84.988673578268,51.3090997168225,31.8868956670179)) ;
#16842 = CARTESIAN_POINT('Ctrl Pts',(85.319725664392,51.4549098432584,31.9079382282172)) ;
#16843 = CARTESIAN_POINT('Ctrl Pts',(85.5148267572544,51.7061453200447,31.9289807894165)) ;
#16844 = CARTESIAN_POINT('Ctrl Pts',(85.7099278501168,51.9573807968311,31.9500233506158)) ;
#16845 = CARTESIAN_POINT('Ctrl Pts',(85.7690779497176,52.3140416239679,31.9710659118151)) ;
#16846 = CARTESIAN_POINT('Ctrl Pts',(85.6656159439665,52.6149428285566,31.9921084730144)) ;
#16847 = CARTESIAN_POINT('Ctrl Pts',(85.5707356449191,52.8908856354625,32.0114056486762)) ;
#16848 = CARTESIAN_POINT('Ctrl Pts',(85.3391003580094,53.1199352145346,32.0307028243381)) ;
#16849 = CARTESIAN_POINT('Ctrl Pts',(85.0634162962529,53.2161025497301,32.05)) ;
#16850 = CARTESIAN_POINT('',(84.3201226220477,51.6988956497206,26.5)) ;
#16851 = CARTESIAN_POINT('Ctrl Pts',(84.3191917355919,51.698168494003,26.5)) ;
#16852 = CARTESIAN_POINT('Ctrl Pts',(84.300816180799,51.7074226812205,26.5)) ;
#16853 = CARTESIAN_POINT('Ctrl Pts',(84.2828934982845,51.7174706610443,26.5)) ;
#16854 = CARTESIAN_POINT('Ctrl Pts',(84.2654813313523,51.7282988497271,26.5)) ;
#16855 = CARTESIAN_POINT('Ctrl Pts',(84.2371864517476,51.7458947237105,26.5)) ;
#16856 = CARTESIAN_POINT('Ctrl Pts',(84.2102385230316,51.7655481374333,26.5)) ;
#16857 = CARTESIAN_POINT('Ctrl Pts',(84.1847000527494,51.7870133766027,26.5)) ;
#16858 = CARTESIAN_POINT('Ctrl Pts',(84.1766854424536,51.793749705167,26.5)) ;
#16859 = CARTESIAN_POINT('Ctrl Pts',(84.1688097413242,51.8006648199525,26.5)) ;
#16860 = CARTESIAN_POINT('Ctrl Pts',(84.1610751954445,51.8077520287958,26.5)) ;
#16861 = CARTESIAN_POINT('Ctrl Pts',(84.1544687104645,51.8138055889534,26.5)) ;
#16862 = CARTESIAN_POINT('Ctrl Pts',(84.1479657078829,51.8199844792118,26.5)) ;
#16863 = CARTESIAN_POINT('Ctrl Pts',(84.1415771515967,51.8262746779352,26.5)) ;
#16864 = CARTESIAN_POINT('Ctrl Pts',(84.1161683064708,51.8512923310664,26.5)) ;
#16865 = CARTESIAN_POINT('Ctrl Pts',(84.0925275072523,51.8781034129898,26.5)) ;
#16866 = CARTESIAN_POINT('Ctrl Pts',(84.0707277650994,51.9064245173419,26.5)) ;
#16867 = CARTESIAN_POINT('Ctrl Pts',(84.0550145507544,51.9268383176543,26.5)) ;
#16868 = CARTESIAN_POINT('Ctrl Pts',(84.0402580944232,51.9480378802971,26.5)) ;
#16869 = CARTESIAN_POINT('Ctrl Pts',(84.0264932335582,51.9699317066184,26.5)) ;
#16870 = CARTESIAN_POINT('Ctrl Pts',(84.0220799558424,51.976951286167,26.5)) ;
#16871 = CARTESIAN_POINT('Ctrl Pts',(84.0177694943993,51.9840412354974,26.5)) ;
#16872 = CARTESIAN_POINT('Ctrl Pts',(84.0135690504379,51.9911877939304,26.5)) ;
#16873 = CARTESIAN_POINT('Ctrl Pts',(83.9944337627959,52.0237442218985,26.5)) ;
#16874 = CARTESIAN_POINT('Ctrl Pts',(83.9775429300529,52.0575290164857,26.5)) ;
#16875 = CARTESIAN_POINT('Ctrl Pts',(83.9629762129376,52.0922399248873,26.5)) ;
#16876 = CARTESIAN_POINT('Ctrl Pts',(83.9482943003256,52.1272253316746,26.5)) ;
#16877 = CARTESIAN_POINT('Ctrl Pts',(83.9359725208531,52.1631526026432,26.5)) ;
#16878 = CARTESIAN_POINT('Ctrl Pts',(83.9261260215936,52.1997538001073,26.5)) ;
#16879 = CARTESIAN_POINT('Ctrl Pts',(83.9209993423921,52.2188105829134,26.5)) ;
#16880 = CARTESIAN_POINT('Ctrl Pts',(83.9165443118937,52.2380506443706,26.5)) ;
#16881 = CARTESIAN_POINT('Ctrl Pts',(83.9127819868296,52.2574390790074,26.5)) ;
#16882 = CARTESIAN_POINT('Ctrl Pts',(83.9109170346052,52.2670497595544,26.5)) ;
#16883 = CARTESIAN_POINT('Ctrl Pts',(83.9092220495422,52.2767000188718,26.5)) ;
#16884 = CARTESIAN_POINT('Ctrl Pts',(83.9077033081333,52.2863606526602,26.5)) ;
#16885 = CARTESIAN_POINT('Ctrl Pts',(83.901448178839,52.3261491993201,26.5)) ;
#16886 = CARTESIAN_POINT('Ctrl Pts',(83.8981611108834,52.3661937690171,26.5)) ;
#16887 = CARTESIAN_POINT('Ctrl Pts',(83.8979520164386,52.4061772604385,26.5)) ;
#16888 = CARTESIAN_POINT('Ctrl Pts',(83.8977552168724,52.4438096986319,26.5)) ;
#16889 = CARTESIAN_POINT('Ctrl Pts',(83.9002842209716,52.4813894674705,26.5)) ;
#16890 = CARTESIAN_POINT('Ctrl Pts',(83.9053641490143,52.5187218857782,26.5)) ;
#16891 = CARTESIAN_POINT('Ctrl Pts',(83.9076860678112,52.5357856794139,26.5)) ;
#16892 = CARTESIAN_POINT('Ctrl Pts',(83.9105416295862,52.5527979619798,26.5)) ;
#16893 = CARTESIAN_POINT('Ctrl Pts',(83.9139175930541,52.5697406004266,26.5)) ;
#16894 = CARTESIAN_POINT('Ctrl Pts',(83.9157766295873,52.5790703766937,26.5)) ;
#16895 = CARTESIAN_POINT('Ctrl Pts',(83.9177935077873,52.5883790360894,26.5)) ;
#16896 = CARTESIAN_POINT('Ctrl Pts',(83.9199662851238,52.5976635435118,26.5)) ;
#16897 = CARTESIAN_POINT('Ctrl Pts',(83.9218283515739,52.6056203504461,26.5)) ;
#16898 = CARTESIAN_POINT('Ctrl Pts',(83.9238028858573,52.6135505871988,26.5)) ;
#16899 = CARTESIAN_POINT('Ctrl Pts',(83.9258870491201,52.6214491569347,26.5)) ;
#16900 = CARTESIAN_POINT('Ctrl Pts',(83.9359905736557,52.6597395320452,26.5)) ;
#16901 = CARTESIAN_POINT('Ctrl Pts',(83.9486718000006,52.6973087601356,26.5)) ;
#16902 = CARTESIAN_POINT('Ctrl Pts',(83.9637234370183,52.7339424030372,26.5)) ;
#16903 = CARTESIAN_POINT('Ctrl Pts',(83.9791245442229,52.7714266089717,26.5)) ;
#16904 = CARTESIAN_POINT('Ctrl Pts',(83.9970075859867,52.8079323713265,26.5)) ;
#16905 = CARTESIAN_POINT('Ctrl Pts',(84.017204939325,52.8432325426417,26.5)) ;
#16906 = CARTESIAN_POINT('Ctrl Pts',(84.0269030196574,52.8601824811523,26.5)) ;
#16907 = CARTESIAN_POINT('Ctrl Pts',(84.0371354640833,52.8768543934362,26.5)) ;
#16908 = CARTESIAN_POINT('Ctrl Pts',(84.0478878140445,52.8932221564482,26.5)) ;
#16909 = CARTESIAN_POINT('Ctrl Pts',(84.0527399920078,52.9006083835783,26.5)) ;
#16910 = CARTESIAN_POINT('Ctrl Pts',(84.0576980786753,52.9079326599278,26.5)) ;
#16911 = CARTESIAN_POINT('Ctrl Pts',(84.0627609102679,52.9151925072417,26.5)) ;
#16912 = CARTESIAN_POINT('Ctrl Pts',(84.0674266702075,52.9218829736626,26.5)) ;
#16913 = CARTESIAN_POINT('Ctrl Pts',(84.0721756387589,52.9285104572487,26.5)) ;
#16914 = CARTESIAN_POINT('Ctrl Pts',(84.077005709343,52.9350725962358,26.5)) ;
#16915 = CARTESIAN_POINT('Ctrl Pts',(84.1020890028368,52.9691507852175,26.5)) ;
#16916 = CARTESIAN_POINT('Ctrl Pts',(84.1293595617806,53.0014733682414,26.5)) ;
#16917 = CARTESIAN_POINT('Ctrl Pts',(84.1586216298365,53.0318036918634,26.5)) ;
#16918 = CARTESIAN_POINT('Ctrl Pts',(84.1876858283235,53.0619289223917,26.5)) ;
#16919 = CARTESIAN_POINT('Ctrl Pts',(84.218715233164,53.0900899244461,26.5)) ;
#16920 = CARTESIAN_POINT('Ctrl Pts',(84.2515653891372,53.1160380022807,26.5)) ;
#16921 = CARTESIAN_POINT('Ctrl Pts',(84.2750831177722,53.1346144697293,26.5)) ;
#16922 = CARTESIAN_POINT('Ctrl Pts',(84.2995350324732,53.1520564609265,26.5)) ;
#16923 = CARTESIAN_POINT('Ctrl Pts',(84.3248808714849,53.1682622236805,26.5)) ;
#16924 = CARTESIAN_POINT('Ctrl Pts',(84.3191917355918,51.698168494003,26.5)) ;
#16925 = CARTESIAN_POINT('Ctrl Pts',(84.5014531352299,51.5693465265704,26.5192971756619)) ;
#16926 = CARTESIAN_POINT('Ctrl Pts',(85.0144035932418,51.4807025406976,26.5596369125231)) ;
#16927 = CARTESIAN_POINT('Ctrl Pts',(85.5851072300976,52.0500826073856,26.6210192105835)) ;
#16928 = CARTESIAN_POINT('Ctrl Pts',(85.4162279933292,52.8622720429723,26.6841468941814)) ;
#16929 = CARTESIAN_POINT('Ctrl Pts',(84.6440981710049,53.1652507798167,26.7472745777793)) ;
#16930 = CARTESIAN_POINT('Ctrl Pts',(84.0893208210195,52.7712374725307,26.7990664661529)) ;
#16931 = CARTESIAN_POINT('Ctrl Pts',(84.0119256629849,52.4132474725981,26.8298157933273)) ;
#16932 = CARTESIAN_POINT('Ctrl Pts',(84.0121333942101,52.3001533432303,26.8395225593024)) ;
#16933 = CARTESIAN_POINT('Origin',(84.75,52.3,26.5)) ;
#16934 = CARTESIAN_POINT('',(85.71675,52.3,26.5)) ;
#16935 = CARTESIAN_POINT('Origin',(84.75,52.3,26.5)) ;
#16936 = CARTESIAN_POINT('',(85.1798773779524,51.6988956497206,26.5)) ;
#16937 = CARTESIAN_POINT('Ctrl Pts',(85.1761635223117,53.1694011139097,26.5)) ;
#16938 = CARTESIAN_POINT('Ctrl Pts',(85.1985358633421,53.1552500678604,26.5)) ;
#16939 = CARTESIAN_POINT('Ctrl Pts',(85.2202463454435,53.140146062992,26.5)) ;
#16940 = CARTESIAN_POINT('Ctrl Pts',(85.2412230990218,53.124086385618,26.5)) ;
#16941 = CARTESIAN_POINT('Ctrl Pts',(85.2709792476784,53.1013052557575,26.5)) ;
#16942 = CARTESIAN_POINT('Ctrl Pts',(85.299260215467,53.0766014077599,26.5)) ;
#16943 = CARTESIAN_POINT('Ctrl Pts',(85.3259689576471,53.0501717378542,26.5)) ;
#16944 = CARTESIAN_POINT('Ctrl Pts',(85.3365379879513,53.0397131404302,26.5)) ;
#16945 = CARTESIAN_POINT('Ctrl Pts',(85.3468605118166,53.0289841303707,26.5)) ;
#16946 = CARTESIAN_POINT('Ctrl Pts',(85.3569292400932,53.0179964066639,26.5)) ;
#16947 = CARTESIAN_POINT('Ctrl Pts',(85.3659968469546,53.008101178971,26.5)) ;
#16948 = CARTESIAN_POINT('Ctrl Pts',(85.3748614400538,52.9979924081547,26.5)) ;
#16949 = CARTESIAN_POINT('Ctrl Pts',(85.3834989214389,52.9877012976841,26.5)) ;
#16950 = CARTESIAN_POINT('Ctrl Pts',(85.4103301405326,52.9557332936509,26.5)) ;
#16951 = CARTESIAN_POINT('Ctrl Pts',(85.4350085357348,52.9219718748241,26.5)) ;
#16952 = CARTESIAN_POINT('Ctrl Pts',(85.4573964573398,52.8866925744485,26.5)) ;
#16953 = CARTESIAN_POINT('Ctrl Pts',(85.47039247077,52.8662132164456,26.5)) ;
#16954 = CARTESIAN_POINT('Ctrl Pts',(85.4826157668332,52.8452219775538,26.5)) ;
#16955 = CARTESIAN_POINT('Ctrl Pts',(85.4940314606313,52.8237712759791,26.5)) ;
#16956 = CARTESIAN_POINT('Ctrl Pts',(85.4983243680267,52.8157046724896,26.5)) ;
#16957 = CARTESIAN_POINT('Ctrl Pts',(85.5025030055992,52.8075730922421,26.5)) ;
#16958 = CARTESIAN_POINT('Ctrl Pts',(85.5065652899046,52.7993793320376,26.5)) ;
#16959 = CARTESIAN_POINT('Ctrl Pts',(85.5103912382234,52.7916622692417,26.5)) ;
#16960 = CARTESIAN_POINT('Ctrl Pts',(85.5141117268159,52.7838944289501,26.5)) ;
#16961 = CARTESIAN_POINT('Ctrl Pts',(85.5177221829035,52.7760855289403,26.5)) ;
#16962 = CARTESIAN_POINT('Ctrl Pts',(85.5345633035423,52.7396605942701,26.5)) ;
#16963 = CARTESIAN_POINT('Ctrl Pts',(85.5490381405068,52.702295152328,26.5)) ;
#16964 = CARTESIAN_POINT('Ctrl Pts',(85.5610187828003,52.6642349459369,26.5)) ;
#16965 = CARTESIAN_POINT('Ctrl Pts',(85.5727220868461,52.627055790051,26.5)) ;
#16966 = CARTESIAN_POINT('Ctrl Pts',(85.5820454153636,52.5892125751062,26.5)) ;
#16967 = CARTESIAN_POINT('Ctrl Pts',(85.5888213376671,52.5509364354455,26.5)) ;
#16968 = CARTESIAN_POINT('Ctrl Pts',(85.5920775623131,52.5325425248108,26.5)) ;
#16969 = CARTESIAN_POINT('Ctrl Pts',(85.5947447687977,52.5140487672799,26.5)) ;
#16970 = CARTESIAN_POINT('Ctrl Pts',(85.5968001972194,52.4954820749433,26.5)) ;
#16971 = CARTESIAN_POINT('Ctrl Pts',(85.5978239244134,52.4862347435132,26.5)) ;
#16972 = CARTESIAN_POINT('Ctrl Pts',(85.5986958482688,52.4769693367571,26.5)) ;
#16973 = CARTESIAN_POINT('Ctrl Pts',(85.5994128958565,52.4676892980339,26.5)) ;
#16974 = CARTESIAN_POINT('Ctrl Pts',(85.6000043549324,52.4600346273781,26.5)) ;
#16975 = CARTESIAN_POINT('Ctrl Pts',(85.6004896712265,52.4523798650142,26.5)) ;
#16976 = CARTESIAN_POINT('Ctrl Pts',(85.6008678559599,52.4447271034925,26.5)) ;
#16977 = CARTESIAN_POINT('Ctrl Pts',(85.6026761979484,52.4081343783921,26.5)) ;
#16978 = CARTESIAN_POINT('Ctrl Pts',(85.6020389100667,52.3715841873092,26.5)) ;
#16979 = CARTESIAN_POINT('Ctrl Pts',(85.5988231850837,52.3352753060488,26.5)) ;
#16980 = CARTESIAN_POINT('Ctrl Pts',(85.5958140040931,52.301298521387,26.5)) ;
#16981 = CARTESIAN_POINT('Ctrl Pts',(85.5905459134365,52.2675325087441,26.5)) ;
#16982 = CARTESIAN_POINT('Ctrl Pts',(85.5831173524095,52.2341559873963,26.5)) ;
#16983 = CARTESIAN_POINT('Ctrl Pts',(85.579167991973,52.2164115127345,26.5)) ;
#16984 = CARTESIAN_POINT('Ctrl Pts',(85.5746075077317,52.1987774139026,26.5)) ;
#16985 = CARTESIAN_POINT('Ctrl Pts',(85.5694479139689,52.1812830263565,26.5)) ;
#16986 = CARTESIAN_POINT('Ctrl Pts',(85.5668870334088,52.1725999712483,26.5)) ;
#16987 = CARTESIAN_POINT('Ctrl Pts',(85.564178537469,52.1639513642352,26.5)) ;
#16988 = CARTESIAN_POINT('Ctrl Pts',(85.561323752231,52.1553409885211,26.5)) ;
#16989 = CARTESIAN_POINT('Ctrl Pts',(85.5588931172939,52.148009901141,26.5)) ;
#16990 = CARTESIAN_POINT('Ctrl Pts',(85.5563563430786,52.1407066816808,26.5)) ;
#16991 = CARTESIAN_POINT('Ctrl Pts',(85.5537193745141,52.133446803083,26.5)) ;
#16992 = CARTESIAN_POINT('Ctrl Pts',(85.5409854555251,52.0983888554173,26.5)) ;
#16993 = CARTESIAN_POINT('Ctrl Pts',(85.5258928434259,52.0642593605704,26.5)) ;
#16994 = CARTESIAN_POINT('Ctrl Pts',(85.508587962428,52.0312868386761,26.5)) ;
#16995 = CARTESIAN_POINT('Ctrl Pts',(85.4914700182882,51.9986705041284,26.5)) ;
#16996 = CARTESIAN_POINT('Ctrl Pts',(85.4721863693872,51.9671853904795,26.5)) ;
#16997 = CARTESIAN_POINT('Ctrl Pts',(85.4508457342638,51.9370907524033,26.5)) ;
#16998 = CARTESIAN_POINT('Ctrl Pts',(85.4412665554904,51.9235821610897,26.5)) ;
#16999 = CARTESIAN_POINT('Ctrl Pts',(85.4312725678517,51.9103543233663,26.5)) ;
#17000 = CARTESIAN_POINT('Ctrl Pts',(85.4208721852388,51.8974339258895,26.5)) ;
#17001 = CARTESIAN_POINT('Ctrl Pts',(85.4158879561118,51.8912420170114,26.5)) ;
#17002 = CARTESIAN_POINT('Ctrl Pts',(85.4108093073963,51.8851194961188,26.5)) ;
#17003 = CARTESIAN_POINT('Ctrl Pts',(85.4056404831104,51.8790734146626,26.5)) ;
#17004 = CARTESIAN_POINT('Ctrl Pts',(85.3826093912735,51.8521334667038,26.5)) ;
#17005 = CARTESIAN_POINT('Ctrl Pts',(85.3578991214674,51.8268335867781,26.5)) ;
#17006 = CARTESIAN_POINT('Ctrl Pts',(85.3316223570636,51.8033912601801,26.5)) ;
#17007 = CARTESIAN_POINT('Ctrl Pts',(85.3062984575833,51.7807990142998,26.5)) ;
#17008 = CARTESIAN_POINT('Ctrl Pts',(85.2795187383892,51.7599316341875,26.5)) ;
#17009 = CARTESIAN_POINT('Ctrl Pts',(85.2513665981943,51.741027670526,26.5)) ;
#17010 = CARTESIAN_POINT('Ctrl Pts',(85.2284341168372,51.7256286709742,26.5)) ;
#17011 = CARTESIAN_POINT('Ctrl Pts',(85.2045904738039,51.7115331865253,26.5)) ;
#17012 = CARTESIAN_POINT('Ctrl Pts',(85.1798773779524,51.6988956497206,26.5)) ;
#17013 = CARTESIAN_POINT('Origin',(84.75,52.3,26.5)) ;
#17014 = CARTESIAN_POINT('Origin',(84.75,52.3,26.5)) ;
#17015 = CARTESIAN_POINT('Origin',(84.75,52.3,25.7604774406976)) ;
#17016 = CARTESIAN_POINT('Ctrl Pts',(85.1798773779524,51.6988956497206,26.5)) ;
#17017 = CARTESIAN_POINT('Ctrl Pts',(85.3785638722607,51.8409855034509,26.5210425611993)) ;
#17018 = CARTESIAN_POINT('Ctrl Pts',(85.6206111574732,52.3353302012154,26.5631276835978)) ;
#17019 = CARTESIAN_POINT('Ctrl Pts',(85.1965387349045,53.0492386288041,26.6262553671958)) ;
#17020 = CARTESIAN_POINT('Ctrl Pts',(84.3675652084279,53.0831821640869,26.6893830507936)) ;
#17021 = CARTESIAN_POINT('Ctrl Pts',(84.0256471893491,52.6053061792988,26.7341237419609)) ;
#17022 = CARTESIAN_POINT('Ctrl Pts',(84.0100192177397,52.3312588893219,26.7578218719289)) ;
#17023 = CARTESIAN_POINT('Ctrl Pts',(84.010254873815,52.3005215753354,26.7604774406976)) ;
#17024 = CARTESIAN_POINT('Ctrl Pts',(85.3123598851629,51.5136432603077,26.3685084761921)) ;
#17025 = CARTESIAN_POINT('Ctrl Pts',(85.5722789222031,51.6995233226808,26.3895510373913)) ;
#17026 = CARTESIAN_POINT('Ctrl Pts',(85.8889219708895,52.3462185007104,26.4316361597899)) ;
#17027 = CARTESIAN_POINT('Ctrl Pts',(85.3341560513787,53.2801440384254,26.4947638433878)) ;
#17028 = CARTESIAN_POINT('Ctrl Pts',(84.2497038771959,53.3245485211515,26.5578915269856)) ;
#17029 = CARTESIAN_POINT('Ctrl Pts',(83.6185883054696,52.4424804272665,26.6210192105836)) ;
#17030 = CARTESIAN_POINT('Ctrl Pts',(84.01154584563,51.4309028921684,26.6841468941814)) ;
#17031 = CARTESIAN_POINT('Ctrl Pts',(85.0731334617142,51.2063834341436,26.7472745777793)) ;
#17032 = CARTESIAN_POINT('Ctrl Pts',(85.8421357429227,51.9717988075231,26.8104022613771)) ;
#17033 = CARTESIAN_POINT('Ctrl Pts',(85.622441895197,53.0344000170724,26.873529944975)) ;
#17034 = CARTESIAN_POINT('Ctrl Pts',(84.6129062855387,53.4321114217142,26.9366576285728)) ;
#17035 = CARTESIAN_POINT('Ctrl Pts',(83.7274888206984,52.8049270108724,26.9997853121707)) ;
#17036 = CARTESIAN_POINT('Ctrl Pts',(83.7677572516237,51.7206200598891,27.0629129957686)) ;
#17037 = CARTESIAN_POINT('Ctrl Pts',(84.6972605634971,51.1608347951476,27.1260406793665)) ;
#17038 = CARTESIAN_POINT('Ctrl Pts',(85.6745086642054,51.6323445107387,27.1891683629643)) ;
#17039 = CARTESIAN_POINT('Ctrl Pts',(85.8147908759896,52.7082898034173,27.2522960465622)) ;
#17040 = CARTESIAN_POINT('Ctrl Pts',(84.9911078932332,53.4146061239167,27.3154237301601)) ;
#17041 = CARTESIAN_POINT('Ctrl Pts',(83.9491477911621,53.1118594344693,27.3785514137579)) ;
#17042 = CARTESIAN_POINT('Ctrl Pts',(83.6322065542242,52.074128788224,27.4416790973558)) ;
#17043 = CARTESIAN_POINT('Ctrl Pts',(84.3272140762793,51.2408814903139,27.5048067809536)) ;
#17044 = CARTESIAN_POINT('Ctrl Pts',(85.4049735927635,51.3664639428714,27.5679344645516)) ;
#17045 = CARTESIAN_POINT('Ctrl Pts',(85.8897794667379,52.3371852294877,27.6310621481493)) ;
#17046 = CARTESIAN_POINT('Ctrl Pts',(85.3427324518969,53.2742423778523,27.6941898317473)) ;
#17047 = CARTESIAN_POINT('Ctrl Pts',(84.2590792708789,53.3293088996161,27.7573175153451)) ;
#17048 = CARTESIAN_POINT('Ctrl Pts',(83.6198611629693,52.4525325590144,27.820445198943)) ;
#17049 = CARTESIAN_POINT('Ctrl Pts',(84.0037681905173,51.437667083614,27.8835728825408)) ;
#17050 = CARTESIAN_POINT('Ctrl Pts',(85.0632457725477,51.2034795676857,27.9467005661387)) ;
#17051 = CARTESIAN_POINT('Ctrl Pts',(85.839139061397,51.9619821345739,28.0098282497366)) ;
#17052 = CARTESIAN_POINT('Ctrl Pts',(85.6290246908954,53.0264953992789,28.0729559333345)) ;
#17053 = CARTESIAN_POINT('Ctrl Pts',(84.623121142821,53.4333056639836,28.1360836169323)) ;
#17054 = CARTESIAN_POINT('Ctrl Pts',(83.7320821968977,52.8141238357924,28.1992113005302)) ;
#17055 = CARTESIAN_POINT('Ctrl Pts',(83.7625736468539,51.7295009469655,28.2623389841281)) ;
#17056 = CARTESIAN_POINT('Ctrl Pts',(84.6869913012024,51.1613561240314,28.3254666677259)) ;
#17057 = CARTESIAN_POINT('Ctrl Pts',(85.6684513129697,51.6240361266255,28.3885943513238)) ;
#17058 = CARTESIAN_POINT('Ctrl Pts',(85.818428861758,52.6986724717933,28.4517220349216)) ;
#17059 = CARTESIAN_POINT('Ctrl Pts',(85.0011478863907,53.4123869432734,28.5148497185195)) ;
#17060 = CARTESIAN_POINT('Ctrl Pts',(83.9565004080862,53.1190472330921,28.5779774021174)) ;
#17061 = CARTESIAN_POINT('Ctrl Pts',(83.6302154447458,52.0842164922485,28.6411050857152)) ;
#17062 = CARTESIAN_POINT('Ctrl Pts',(84.3176817895697,51.2447365554831,28.7042327693131)) ;
#17063 = CARTESIAN_POINT('Ctrl Pts',(85.3965298062611,51.3605963689557,28.767360452911)) ;
#17064 = CARTESIAN_POINT('Ctrl Pts',(85.890068413398,52.3269069726244,28.8304881365088)) ;
#17065 = CARTESIAN_POINT('Ctrl Pts',(85.351492548107,53.2688584452722,28.8936158201067)) ;
#17066 = CARTESIAN_POINT('Ctrl Pts',(84.2683799193525,53.3336934121491,28.9567435037046)) ;
#17067 = CARTESIAN_POINT('Ctrl Pts',(83.6212824012761,52.4627161784649,29.0198711873024)) ;
#17068 = CARTESIAN_POINT('Ctrl Pts',(83.9960233581859,51.4444304844127,29.0829988709003)) ;
#17069 = CARTESIAN_POINT('Ctrl Pts',(85.0533463380197,51.2006997809454,29.1461265544982)) ;
#17070 = CARTESIAN_POINT('Ctrl Pts',(85.8360470741805,51.9521757267418,29.209254238096)) ;
#17071 = CARTESIAN_POINT('Ctrl Pts',(85.6355393556322,53.0185402020971,29.2723819216939)) ;
#17072 = CARTESIAN_POINT('Ctrl Pts',(84.6333446732919,53.4344035909473,29.3355096052918)) ;
#17073 = CARTESIAN_POINT('Ctrl Pts',(83.7367591364786,52.8232809234949,29.3986372888896)) ;
#17074 = CARTESIAN_POINT('Ctrl Pts',(83.7574699189085,51.7384271992591,29.4617649724875)) ;
#17075 = CARTESIAN_POINT('Ctrl Pts',(84.6767273578161,51.1619705222136,29.5248926560853)) ;
#17076 = CARTESIAN_POINT('Ctrl Pts',(85.6623191969598,51.6157824503406,29.5880203396833)) ;
#17077 = CARTESIAN_POINT('Ctrl Pts',(85.8219800344285,52.6890228504728,29.6511480232811)) ;
#17078 = CARTESIAN_POINT('Ctrl Pts',(85.011167438299,53.4100772682907,29.714275706879)) ;
#17079 = CARTESIAN_POINT('Ctrl Pts',(83.9639175462777,53.126168474558,29.7774033904768)) ;
#17080 = CARTESIAN_POINT('Ctrl Pts',(83.6283153654585,52.0943217244413,29.8405310740747)) ;
#17081 = CARTESIAN_POINT('Ctrl Pts',(84.3081846521447,51.2486774182948,29.9036587576725)) ;
#17082 = CARTESIAN_POINT('Ctrl Pts',(85.3880334569927,51.3548051628574,29.9667864412704)) ;
#17083 = CARTESIAN_POINT('Ctrl Pts',(85.8902646758111,52.3166265300249,30.0299141248683)) ;
#17084 = CARTESIAN_POINT('Ctrl Pts',(85.3602037440254,53.2633957458814,30.0930418084661)) ;
#17085 = CARTESIAN_POINT('Ctrl Pts',(84.2777197225921,53.3379938882152,30.156169492064)) ;
#17086 = CARTESIAN_POINT('Ctrl Pts',(83.6227954016365,52.4728865692609,30.2192971756619)) ;
#17087 = CARTESIAN_POINT('Ctrl Pts',(83.9883398224533,51.4512634411337,30.2824248592598)) ;
#17088 = CARTESIAN_POINT('Ctrl Pts',(85.0434222421183,51.198009364737,30.3455525428576)) ;
#17089 = CARTESIAN_POINT('Ctrl Pts',(85.8328667938476,51.9423975962189,30.4086802264555)) ;
#17090 = CARTESIAN_POINT('Ctrl Pts',(85.6419820280726,53.0105265892964,30.4718079100534)) ;
#17091 = CARTESIAN_POINT('Ctrl Pts',(84.6435776875471,53.4354092934174,30.5349355936512)) ;
#17092 = CARTESIAN_POINT('Ctrl Pts',(83.7415184502553,52.8323954698803,30.5980632772491)) ;
#17093 = CARTESIAN_POINT('Ctrl Pts',(83.7524468812573,51.747399105686,30.6611909608469)) ;
#17094 = CARTESIAN_POINT('Ctrl Pts',(84.6664693715499,51.1626774404569,30.7243186444448)) ;
#17095 = CARTESIAN_POINT('Ctrl Pts',(85.6561129110516,51.6075843975507,30.7874463280427)) ;
#17096 = CARTESIAN_POINT('Ctrl Pts',(85.8254440585195,52.67934160617,30.8505740116405)) ;
#17097 = CARTESIAN_POINT('Ctrl Pts',(85.0211657560265,53.4076773391265,30.9137016952384)) ;
#17098 = CARTESIAN_POINT('Ctrl Pts',(83.9713985949548,53.1332225655791,30.9768293788363)) ;
#17099 = CARTESIAN_POINT('Ctrl Pts',(83.6265064688367,52.1044436470692,31.0399570624342)) ;
#17100 = CARTESIAN_POINT('Ctrl Pts',(84.2987234489242,51.2527038135746,31.103084746032)) ;
#17101 = CARTESIAN_POINT('Ctrl Pts',(85.379485205345,51.3490906723475,31.1662124296299)) ;
#17102 = CARTESIAN_POINT('Ctrl Pts',(85.8903683017345,52.3063449925798,31.2293401132277)) ;
#17103 = CARTESIAN_POINT('Ctrl Pts',(85.3688652011076,53.2578542033979,31.2924677968256)) ;
#17104 = CARTESIAN_POINT('Ctrl Pts',(84.2870981863241,53.3422110355567,31.3555954804235)) ;
#17105 = CARTESIAN_POINT('Ctrl Pts',(83.6243995029531,52.483040758174,31.4187231640213)) ;
#17106 = CARTESIAN_POINT('Ctrl Pts',(83.9807193000769,51.4581697543765,31.4818508476192)) ;
#17107 = CARTESIAN_POINT('Ctrl Pts',(85.0334720753324,51.195399697593,31.5449785312171)) ;
#17108 = CARTESIAN_POINT('Ctrl Pts',(85.8296029766522,51.9326664778211,31.608106214815)) ;
#17109 = CARTESIAN_POINT('Ctrl Pts',(85.6483430569928,53.0024188060892,31.6712338984128)) ;
#17110 = CARTESIAN_POINT('Ctrl Pts',(84.6538378769964,53.4363965712052,31.7343615820107)) ;
#17111 = CARTESIAN_POINT('Ctrl Pts',(83.7463221504495,52.8413167917181,31.7974892656085)) ;
#17112 = CARTESIAN_POINT('Ctrl Pts',(83.7475813626246,51.7567203683836,31.8606169492064)) ;
#17113 = CARTESIAN_POINT('Ctrl Pts',(84.6560601317181,51.1628562405876,31.9237446328043)) ;
#17114 = CARTESIAN_POINT('Ctrl Pts',(85.6501671264575,51.6007299877531,31.9868723164022)) ;
#17115 = CARTESIAN_POINT('Ctrl Pts',(85.7681319415962,52.3110551076506,32.0289574388007)) ;
#17116 = CARTESIAN_POINT('Ctrl Pts',(85.6645587247976,52.6133494876276,32.05)) ;
#17117 = CARTESIAN_POINT('Ctrl Pts',(85.2681990494261,51.5753940567787,26.412338984128)) ;
#17118 = CARTESIAN_POINT('Ctrl Pts',(85.507707238889,51.7466773829375,26.4333815453273)) ;
#17119 = CARTESIAN_POINT('Ctrl Pts',(85.799485033084,52.3425890675454,26.4754666677259)) ;
#17120 = CARTESIAN_POINT('Ctrl Pts',(85.288283612554,53.2031755685516,26.5385943513238)) ;
#17121 = CARTESIAN_POINT('Ctrl Pts',(84.2889909876065,53.2440930687966,26.6017220349216)) ;
#17122 = CARTESIAN_POINT('Ctrl Pts',(83.7074354784476,52.4312917651477,26.6648497185195)) ;
#17123 = CARTESIAN_POINT('Ctrl Pts',(84.0695349616227,51.4991511005327,26.7279774021173)) ;
#17124 = CARTESIAN_POINT('Ctrl Pts',(85.0477585299305,51.2922626420993,26.7911050857153)) ;
#17125 = CARTESIAN_POINT('Ctrl Pts',(85.7563728206055,51.9975716966143,26.8542327693131)) ;
#17126 = CARTESIAN_POINT('Ctrl Pts',(85.5539310283299,52.9767292632104,26.917360452911)) ;
#17127 = CARTESIAN_POINT('Ctrl Pts',(84.6236719414196,53.3432093007606,26.9804881365088)) ;
#17128 = CARTESIAN_POINT('Ctrl Pts',(83.807784285257,52.7652762474119,27.0436158201067)) ;
#17129 = CARTESIAN_POINT('Ctrl Pts',(83.8448905283904,51.7661174416184,27.1067435037046)) ;
#17130 = CARTESIAN_POINT('Ctrl Pts',(84.7014020708374,51.2502908335599,27.1698711873024)) ;
#17131 = CARTESIAN_POINT('Ctrl Pts',(85.6019091130382,51.6847739694679,27.2329988709003)) ;
#17132 = CARTESIAN_POINT('Ctrl Pts',(85.7311752835383,52.6762277388613,27.2961265544982)) ;
#17133 = CARTESIAN_POINT('Ctrl Pts',(84.9721742417605,53.3270786539669,27.359254238096)) ;
#17134 = CARTESIAN_POINT('Ctrl Pts',(84.0120368836758,53.0481059696989,27.4223819216939)) ;
#17135 = CARTESIAN_POINT('Ctrl Pts',(83.7199843172707,52.0918659379462,27.4855096052918)) ;
#17136 = CARTESIAN_POINT('Ctrl Pts',(84.3604144880119,51.3240516448113,27.5486372888896)) ;
#17137 = CARTESIAN_POINT('Ctrl Pts',(85.3535400143643,51.4397723945604,27.6117649724875)) ;
#17138 = CARTESIAN_POINT('Ctrl Pts',(85.8002751917446,52.3342651584539,27.6748926560853)) ;
#17139 = CARTESIAN_POINT('Ctrl Pts',(85.2961865279525,53.197737351887,27.7380203396833)) ;
#17140 = CARTESIAN_POINT('Ctrl Pts',(84.2976301530641,53.2484796256268,27.8011480232811)) ;
#17141 = CARTESIAN_POINT('Ctrl Pts',(83.7086083813586,52.4405545259773,27.864275706879)) ;
#17142 = CARTESIAN_POINT('Ctrl Pts',(84.0623680679795,51.5053841154929,27.9274033904768)) ;
#17143 = CARTESIAN_POINT('Ctrl Pts',(85.0386472983824,51.2895868096337,27.9905310740747)) ;
#17144 = CARTESIAN_POINT('Ctrl Pts',(85.7536114616269,51.9885259045423,28.0536587576725)) ;
#17145 = CARTESIAN_POINT('Ctrl Pts',(85.5599968921362,52.9694453769754,28.1167864412704)) ;
#17146 = CARTESIAN_POINT('Ctrl Pts',(84.6330846493196,53.3443097619158,28.1799141248683)) ;
#17147 = CARTESIAN_POINT('Ctrl Pts',(83.8120169541277,52.7737508667029,28.2430418084662)) ;
#17148 = CARTESIAN_POINT('Ctrl Pts',(83.840113980249,51.7743009329421,28.306169492064)) ;
#17149 = CARTESIAN_POINT('Ctrl Pts',(84.6919392302261,51.2507712236786,28.3692971756619)) ;
#17150 = CARTESIAN_POINT('Ctrl Pts',(85.5963274317427,51.6771180237589,28.4324248592598)) ;
#17151 = CARTESIAN_POINT('Ctrl Pts',(85.7345275866039,52.6673656342962,28.4955525428576)) ;
#17152 = CARTESIAN_POINT('Ctrl Pts',(84.9814258172154,53.3250337405045,28.5586802264555)) ;
#17153 = CARTESIAN_POINT('Ctrl Pts',(84.0188121164073,53.0547293269334,28.6218079100534)) ;
#17154 = CARTESIAN_POINT('Ctrl Pts',(83.7181495650662,52.101161477643,28.6849355936512)) ;
#17155 = CARTESIAN_POINT('Ctrl Pts',(84.3516307499784,51.3276039805287,28.7480632772491)) ;
#17156 = CARTESIAN_POINT('Ctrl Pts',(85.3457592991063,51.4343655878059,28.8111909608469)) ;
#17157 = CARTESIAN_POINT('Ctrl Pts',(85.8005414480841,52.324794029597,28.8743186444448)) ;
#17158 = CARTESIAN_POINT('Ctrl Pts',(85.3042587138404,53.19277620722,28.9374463280427)) ;
#17159 = CARTESIAN_POINT('Ctrl Pts',(84.3062004428825,53.2525198324174,29.0005740116406)) ;
#17160 = CARTESIAN_POINT('Ctrl Pts',(83.7099180130712,52.4499384490811,29.0637016952384)) ;
#17161 = CARTESIAN_POINT('Ctrl Pts',(84.0552314196198,51.511616401894,29.1268293788363)) ;
#17162 = CARTESIAN_POINT('Ctrl Pts',(85.0295252438092,51.2870253131891,29.1899570624341)) ;
#17163 = CARTESIAN_POINT('Ctrl Pts',(85.7507622810954,51.9794895714913,29.253084746032)) ;
#17164 = CARTESIAN_POINT('Ctrl Pts',(85.5659999751495,52.9621148832358,29.3162124296299)) ;
#17165 = CARTESIAN_POINT('Ctrl Pts',(84.6425053493224,53.3453214711857,29.3793401132277)) ;
#17166 = CARTESIAN_POINT('Ctrl Pts',(83.8163266243389,52.7821888692492,29.4424677968256)) ;
#17167 = CARTESIAN_POINT('Ctrl Pts',(83.8354110363875,51.7825262270562,29.5055954804235)) ;
#17168 = CARTESIAN_POINT('Ctrl Pts',(84.6824812908417,51.2513373745766,29.5687231640214)) ;
#17169 = CARTESIAN_POINT('Ctrl Pts',(85.5906768567795,51.6695124897975,29.6318508476192)) ;
#17170 = CARTESIAN_POINT('Ctrl Pts',(85.7377998938059,52.6584737756706,29.6949785312171)) ;
#17171 = CARTESIAN_POINT('Ctrl Pts',(84.9906585566257,53.3229054390162,29.7581062148149)) ;
#17172 = CARTESIAN_POINT('Ctrl Pts',(84.0256468036988,53.0612913535924,29.8212338984128)) ;
#17173 = CARTESIAN_POINT('Ctrl Pts',(83.71639869466,52.110473169061,29.8843615820107)) ;
#17174 = CARTESIAN_POINT('Ctrl Pts',(84.3428794010367,51.3312353763962,29.9474892656085)) ;
#17175 = CARTESIAN_POINT('Ctrl Pts',(85.3379301487158,51.4290291518787,30.0106169492064)) ;
#17176 = CARTESIAN_POINT('Ctrl Pts',(85.8007222984588,52.3153208866449,30.0737446328043)) ;
#17177 = CARTESIAN_POINT('Ctrl Pts',(85.3122858394649,53.1877424811199,30.1368723164021)) ;
#17178 = CARTESIAN_POINT('Ctrl Pts',(84.3148068127324,53.2564826019327,30.2)) ;
#17179 = CARTESIAN_POINT('Ctrl Pts',(83.7113122009735,52.4593101823462,30.2631276835979)) ;
#17180 = CARTESIAN_POINT('Ctrl Pts',(84.0481512543769,51.5179127821498,30.3262553671957)) ;
#17181 = CARTESIAN_POINT('Ctrl Pts',(85.0203804644637,51.2845461692128,30.3893830507936)) ;
#17182 = CARTESIAN_POINT('Ctrl Pts',(85.7478317409044,51.9704792951971,30.4525107343915)) ;
#17183 = CARTESIAN_POINT('Ctrl Pts',(85.5719367192567,52.9547305611222,30.5156384179893)) ;
#17184 = CARTESIAN_POINT('Ctrl Pts',(84.6519347883698,53.3462481981409,30.5787661015872)) ;
#17185 = CARTESIAN_POINT('Ctrl Pts',(83.8207122000886,52.7905876711508,30.6418937851851)) ;
#17186 = CARTESIAN_POINT('Ctrl Pts',(83.830782446396,51.7907935901891,30.7050214687829)) ;
#17187 = CARTESIAN_POINT('Ctrl Pts',(84.6730288407783,51.2519887801469,30.7681491523808)) ;
#17188 = CARTESIAN_POINT('Ctrl Pts',(85.5849579363108,51.6619582113453,30.8312768359787)) ;
#17189 = CARTESIAN_POINT('Ctrl Pts',(85.7409918960066,52.6495527773432,30.8944045195766)) ;
#17190 = CARTESIAN_POINT('Ctrl Pts',(84.9998717293271,53.320693970801,30.9575322031744)) ;
#17191 = CARTESIAN_POINT('Ctrl Pts',(84.0325403827313,53.0677915029774,31.0206598867723)) ;
#17192 = CARTESIAN_POINT('Ctrl Pts',(83.7147318465533,52.1198002402525,31.0837875703701)) ;
#17193 = CARTESIAN_POINT('Ctrl Pts',(84.3341611644685,51.3349455880624,31.146915253968)) ;
#17194 = CARTESIAN_POINT('Ctrl Pts',(85.3300531717214,51.4237634072403,31.2100429375659)) ;
#17195 = CARTESIAN_POINT('Ctrl Pts',(85.8008177868754,52.3058467348228,31.2731706211637)) ;
#17196 = CARTESIAN_POINT('Ctrl Pts',(85.32026713213,53.1826361032949,31.3362983047616)) ;
#17197 = CARTESIAN_POINT('Ctrl Pts',(84.323448807155,53.2603685863375,31.3994259883594)) ;
#17198 = CARTESIAN_POINT('Ctrl Pts',(83.712790335882,52.4686669860253,31.4625536719573)) ;
#17199 = CARTESIAN_POINT('Ctrl Pts',(84.0411291541956,51.5242767584075,31.5256813555552)) ;
#17200 = CARTESIAN_POINT('Ctrl Pts',(85.0112116615207,51.2821414332617,31.5888090391531)) ;
#17201 = CARTESIAN_POINT('Ctrl Pts',(85.7448242238094,51.9615123392732,31.6519367227509)) ;
#17202 = CARTESIAN_POINT('Ctrl Pts',(85.5777982311225,52.9472594635888,31.7150644063488)) ;
#17203 = CARTESIAN_POINT('Ctrl Pts',(84.6613892686054,53.3471579472617,31.7781920899466)) ;
#17204 = CARTESIAN_POINT('Ctrl Pts',(83.825138676692,52.7988084219867,31.8413197735445)) ;
#17205 = CARTESIAN_POINT('Ctrl Pts',(83.8262990058147,51.7993828754435,31.9044474571424)) ;
#17206 = CARTESIAN_POINT('Ctrl Pts',(84.6634370147458,51.2521535395124,31.9675751407403)) ;
#17207 = CARTESIAN_POINT('Ctrl Pts',(85.5794790605837,51.6556420626739,32.0307028243381)) ;
#17208 = CARTESIAN_POINT('Ctrl Pts',(85.6881803685599,52.3101869753284,32.0727879467367)) ;
#17209 = CARTESIAN_POINT('Ctrl Pts',(85.5927405196179,52.5887428689543,32.093830507936)) ;
#17210 = CARTESIAN_POINT('Ctrl Pts',(85.2240382136892,51.6371448532496,26.456169492064)) ;
#17211 = CARTESIAN_POINT('Ctrl Pts',(85.4431355555749,51.7938314431942,26.4772120532633)) ;
#17212 = CARTESIAN_POINT('Ctrl Pts',(85.7100480952787,52.3389596343804,26.5192971756619)) ;
#17213 = CARTESIAN_POINT('Ctrl Pts',(85.2424111737292,53.1262070986779,26.5824248592598)) ;
#17214 = CARTESIAN_POINT('Ctrl Pts',(84.3282780980173,53.1636376164417,26.6455525428576)) ;
#17215 = CARTESIAN_POINT('Ctrl Pts',(83.7962826514255,52.420103103029,26.7086802264555)) ;
#17216 = CARTESIAN_POINT('Ctrl Pts',(84.1275240776153,51.567399308897,26.7718079100533)) ;
#17217 = CARTESIAN_POINT('Ctrl Pts',(85.022383598147,51.3781418500553,26.8349355936512)) ;
#17218 = CARTESIAN_POINT('Ctrl Pts',(85.6706098982882,52.0233445857054,26.8980632772491)) ;
#17219 = CARTESIAN_POINT('Ctrl Pts',(85.4854201614629,52.9190585093486,26.9611909608469)) ;
#17220 = CARTESIAN_POINT('Ctrl Pts',(84.6344375973004,53.254307179807,27.0243186444448)) ;
#17221 = CARTESIAN_POINT('Ctrl Pts',(83.8880797498156,52.7256254839516,27.0874463280427)) ;
#17222 = CARTESIAN_POINT('Ctrl Pts',(83.9220238051571,51.8116148233476,27.1505740116406)) ;
#17223 = CARTESIAN_POINT('Ctrl Pts',(84.7055435781776,51.3397468719722,27.2137016952384)) ;
#17224 = CARTESIAN_POINT('Ctrl Pts',(85.529309561871,51.7372034281971,27.2768293788363)) ;
#17225 = CARTESIAN_POINT('Ctrl Pts',(85.6475596910871,52.6441656743055,27.3399570624341)) ;
#17226 = CARTESIAN_POINT('Ctrl Pts',(84.9532405902877,53.239551184017,27.403084746032)) ;
#17227 = CARTESIAN_POINT('Ctrl Pts',(84.0749259761894,52.9843525049285,27.4662124296298)) ;
#17228 = CARTESIAN_POINT('Ctrl Pts',(83.8077620803171,52.1096030876684,27.5293401132278)) ;
#17229 = CARTESIAN_POINT('Ctrl Pts',(84.3936148997444,51.4072217993087,27.5924677968256)) ;
#17230 = CARTESIAN_POINT('Ctrl Pts',(85.3021064359653,51.5130808462494,27.6555954804235)) ;
#17231 = CARTESIAN_POINT('Ctrl Pts',(85.7107709167511,52.3313450874201,27.7187231640213)) ;
#17232 = CARTESIAN_POINT('Ctrl Pts',(85.2496406040083,53.1212323259216,27.7818508476192)) ;
#17233 = CARTESIAN_POINT('Ctrl Pts',(84.336181035249,53.1676503516375,27.8449785312171)) ;
#17234 = CARTESIAN_POINT('Ctrl Pts',(83.7973555997481,52.4285764929403,27.9081062148149)) ;
#17235 = CARTESIAN_POINT('Ctrl Pts',(84.1209679454417,51.5731011473719,27.9712338984128)) ;
#17236 = CARTESIAN_POINT('Ctrl Pts',(85.0140488242173,51.3756940515816,28.0343615820107)) ;
#17237 = CARTESIAN_POINT('Ctrl Pts',(85.6680838618568,52.0150696745107,28.0974892656085)) ;
#17238 = CARTESIAN_POINT('Ctrl Pts',(85.490969093377,52.9123953546719,28.1606169492064)) ;
#17239 = CARTESIAN_POINT('Ctrl Pts',(84.6430481558181,53.255313859848,28.2237446328043)) ;
#17240 = CARTESIAN_POINT('Ctrl Pts',(83.8919517113578,52.7333778976135,28.2868723164021)) ;
#17241 = CARTESIAN_POINT('Ctrl Pts',(83.917654313644,51.8191009189187,28.35)) ;
#17242 = CARTESIAN_POINT('Ctrl Pts',(84.6968871592499,51.3401863233258,28.4131276835978)) ;
#17243 = CARTESIAN_POINT('Ctrl Pts',(85.5242035505155,51.7301999208923,28.4762553671958)) ;
#17244 = CARTESIAN_POINT('Ctrl Pts',(85.6506263114499,52.6360587967991,28.5393830507936)) ;
#17245 = CARTESIAN_POINT('Ctrl Pts',(84.9617037480403,53.2376805377356,28.6025107343915)) ;
#17246 = CARTESIAN_POINT('Ctrl Pts',(84.0811238247283,52.9904114207747,28.6656384179893)) ;
#17247 = CARTESIAN_POINT('Ctrl Pts',(83.8060836853867,52.1181064630375,28.7287661015872)) ;
#17248 = CARTESIAN_POINT('Ctrl Pts',(84.3855797103871,51.4104714055744,28.791893785185)) ;
#17249 = CARTESIAN_POINT('Ctrl Pts',(85.2949887919515,51.508134806656,28.8550214687829)) ;
#17250 = CARTESIAN_POINT('Ctrl Pts',(85.7110144827702,52.3226810865697,28.9181491523808)) ;
#17251 = CARTESIAN_POINT('Ctrl Pts',(85.257024879574,53.1166939691678,28.9812768359787)) ;
#17252 = CARTESIAN_POINT('Ctrl Pts',(84.3440209664122,53.1713462526857,29.0444045195765)) ;
#17253 = CARTESIAN_POINT('Ctrl Pts',(83.7985536248668,52.4371607196973,29.1075322031744)) ;
#17254 = CARTESIAN_POINT('Ctrl Pts',(84.1144394810533,51.5788023193752,29.1706598867723)) ;
#17255 = CARTESIAN_POINT('Ctrl Pts',(85.0057041495988,51.3733508454328,29.2337875703701)) ;
#17256 = CARTESIAN_POINT('Ctrl Pts',(85.6654774880105,52.0068034162407,29.296915253968)) ;
#17257 = CARTESIAN_POINT('Ctrl Pts',(85.4964605946667,52.9056895643745,29.3600429375659)) ;
#17258 = CARTESIAN_POINT('Ctrl Pts',(84.6516660253531,53.2562393514243,29.4231706211637)) ;
#17259 = CARTESIAN_POINT('Ctrl Pts',(83.8958941121992,52.7410968150035,29.4862983047616)) ;
#17260 = CARTESIAN_POINT('Ctrl Pts',(83.9133521538666,51.8266252548534,29.5494259883595)) ;
#17261 = CARTESIAN_POINT('Ctrl Pts',(84.6882352238673,51.3407042269396,29.6125536719573)) ;
#17262 = CARTESIAN_POINT('Ctrl Pts',(85.5190345165994,51.7232425292544,29.6756813555552)) ;
#17263 = CARTESIAN_POINT('Ctrl Pts',(85.6536197531831,52.6279247008683,29.7388090391531)) ;
#17264 = CARTESIAN_POINT('Ctrl Pts',(84.9701496749526,53.2357336097418,29.8019367227509)) ;
#17265 = CARTESIAN_POINT('Ctrl Pts',(84.0873760611197,52.9964142326266,29.8650644063488)) ;
#17266 = CARTESIAN_POINT('Ctrl Pts',(83.8044820238616,52.1266246136808,29.9281920899467)) ;
#17267 = CARTESIAN_POINT('Ctrl Pts',(84.3775741499287,51.4137933344974,29.9913197735445)) ;
#17268 = CARTESIAN_POINT('Ctrl Pts',(85.2878268404389,51.5032531409002,30.0544474571424)) ;
#17269 = CARTESIAN_POINT('Ctrl Pts',(85.7111799211065,52.3140152432647,30.1175751407402)) ;
#17270 = CARTESIAN_POINT('Ctrl Pts',(85.2643679349042,53.1120892163585,30.1807028243381)) ;
#17271 = CARTESIAN_POINT('Ctrl Pts',(84.3518939028729,53.17497131565,30.243830507936)) ;
#17272 = CARTESIAN_POINT('Ctrl Pts',(83.7998290003106,52.4457337954316,30.3069581915338)) ;
#17273 = CARTESIAN_POINT('Ctrl Pts',(84.1079626863004,51.5845621231658,30.3700858751317)) ;
#17274 = CARTESIAN_POINT('Ctrl Pts',(84.9973386868094,51.3710829736887,30.4332135587296)) ;
#17275 = CARTESIAN_POINT('Ctrl Pts',(85.662796687961,51.9985609941751,30.4963412423274)) ;
#17276 = CARTESIAN_POINT('Ctrl Pts',(85.5018914104407,52.898934532948,30.5594689259253)) ;
#17277 = CARTESIAN_POINT('Ctrl Pts',(84.6602918891925,53.2570871028643,30.6225966095231)) ;
#17278 = CARTESIAN_POINT('Ctrl Pts',(83.8999059499221,52.7487798724213,30.6857242931211)) ;
#17279 = CARTESIAN_POINT('Ctrl Pts',(83.9091180115348,51.8341880746922,30.7488519767189)) ;
#17280 = CARTESIAN_POINT('Ctrl Pts',(84.6795883100066,51.3413001198369,30.8119796603168)) ;
#17281 = CARTESIAN_POINT('Ctrl Pts',(85.51380296157,51.71633202514,30.8751073439147)) ;
#17282 = CARTESIAN_POINT('Ctrl Pts',(85.6565397334938,52.6197639485163,30.9382350275125)) ;
#17283 = CARTESIAN_POINT('Ctrl Pts',(84.9785777026277,53.2337106024755,31.0013627111104)) ;
#17284 = CARTESIAN_POINT('Ctrl Pts',(84.0936821705079,53.0023604403756,31.0644903947082)) ;
#17285 = CARTESIAN_POINT('Ctrl Pts',(83.8029572242698,52.1351568334358,31.1276180783061)) ;
#17286 = CARTESIAN_POINT('Ctrl Pts',(84.3695988800129,51.4171873625503,31.190745761904)) ;
#17287 = CARTESIAN_POINT('Ctrl Pts',(85.2806211380976,51.4984361421331,31.2538734455018)) ;
#17288 = CARTESIAN_POINT('Ctrl Pts',(85.7112672720163,52.3053484770657,31.3170011290997)) ;
#17289 = CARTESIAN_POINT('Ctrl Pts',(85.2716690631524,53.1074180031918,31.3801288126976)) ;
#17290 = CARTESIAN_POINT('Ctrl Pts',(84.3597994279858,53.1785261371183,31.4432564962955)) ;
#17291 = CARTESIAN_POINT('Ctrl Pts',(83.8011811688112,52.4542932138767,31.5063841798933)) ;
#17292 = CARTESIAN_POINT('Ctrl Pts',(84.1015390083141,51.5903837624384,31.5695118634912)) ;
#17293 = CARTESIAN_POINT('Ctrl Pts',(84.9889512477094,51.3688831689305,31.632639547089)) ;
#17294 = CARTESIAN_POINT('Ctrl Pts',(85.6600454709664,51.9903582007252,31.6957672306869)) ;
#17295 = CARTESIAN_POINT('Ctrl Pts',(85.5072534052524,52.8921001210884,31.7588949142848)) ;
#17296 = CARTESIAN_POINT('Ctrl Pts',(84.6689406602144,53.2579193233183,31.8220225978826)) ;
#17297 = CARTESIAN_POINT('Ctrl Pts',(83.9039552029347,52.7563000522551,31.8851502814805)) ;
#17298 = CARTESIAN_POINT('Ctrl Pts',(83.9050166490049,51.8420453825035,31.9482779650783)) ;
#17299 = CARTESIAN_POINT('Ctrl Pts',(84.6708138977735,51.3414508384369,32.0114056486762)) ;
#17300 = CARTESIAN_POINT('Ctrl Pts',(85.5087909947098,51.7105541375948,32.0745333322741)) ;
#17301 = CARTESIAN_POINT('Ctrl Pts',(85.6082287955236,52.3093188430062,32.1166184546727)) ;
#17302 = CARTESIAN_POINT('Ctrl Pts',(85.5209223144381,52.5641362502811,32.137661015872)) ;
#17303 = CARTESIAN_POINT('Ctrl Pts',(85.1798773779524,51.6988956497206,26.5)) ;
#17304 = CARTESIAN_POINT('Ctrl Pts',(85.3785638722607,51.8409855034509,26.5210425611993)) ;
#17305 = CARTESIAN_POINT('Ctrl Pts',(85.6206111574732,52.3353302012154,26.5631276835978)) ;
#17306 = CARTESIAN_POINT('Ctrl Pts',(85.1965387349045,53.0492386288041,26.6262553671958)) ;
#17307 = CARTESIAN_POINT('Ctrl Pts',(84.3675652084279,53.0831821640869,26.6893830507936)) ;
#17308 = CARTESIAN_POINT('Ctrl Pts',(83.8851298244034,52.4089144409102,26.7525107343915)) ;
#17309 = CARTESIAN_POINT('Ctrl Pts',(84.1855131936081,51.6356475172613,26.8156384179893)) ;
#17310 = CARTESIAN_POINT('Ctrl Pts',(84.9970086663633,51.464021058011,26.8787661015872)) ;
#17311 = CARTESIAN_POINT('Ctrl Pts',(85.584846975971,52.0491174747966,26.941893785185)) ;
#17312 = CARTESIAN_POINT('Ctrl Pts',(85.4169092945958,52.8613877554865,27.0050214687829)) ;
#17313 = CARTESIAN_POINT('Ctrl Pts',(84.6452032531813,53.1654050588536,27.0681491523808)) ;
#17314 = CARTESIAN_POINT('Ctrl Pts',(83.968375214374,52.685974720491,27.1312768359787)) ;
#17315 = CARTESIAN_POINT('Ctrl Pts',(83.9991570819239,51.8571122050768,27.1944045195765)) ;
#17316 = CARTESIAN_POINT('Ctrl Pts',(84.7096850855178,51.4292029103844,27.2575322031744)) ;
#17317 = CARTESIAN_POINT('Ctrl Pts',(85.4567100107038,51.7896328869262,27.3206598867723)) ;
#17318 = CARTESIAN_POINT('Ctrl Pts',(85.5639440986358,52.6121036097496,27.3837875703701)) ;
#17319 = CARTESIAN_POINT('Ctrl Pts',(84.934306938815,53.1520237140672,27.446915253968)) ;
#17320 = CARTESIAN_POINT('Ctrl Pts',(84.1378150687031,52.9205990401581,27.5100429375658)) ;
#17321 = CARTESIAN_POINT('Ctrl Pts',(83.8955398433635,52.1273402373907,27.5731706211637)) ;
#17322 = CARTESIAN_POINT('Ctrl Pts',(84.4268153114771,51.490391953806,27.6362983047616)) ;
#17323 = CARTESIAN_POINT('Ctrl Pts',(85.2506728575663,51.5863892979384,27.6994259883594)) ;
#17324 = CARTESIAN_POINT('Ctrl Pts',(85.6212666417578,52.3284250163863,27.7625536719573)) ;
#17325 = CARTESIAN_POINT('Ctrl Pts',(85.203094680064,53.0447272999564,27.8256813555552)) ;
#17326 = CARTESIAN_POINT('Ctrl Pts',(84.3747319174341,53.0868210776482,27.8888090391531)) ;
#17327 = CARTESIAN_POINT('Ctrl Pts',(83.8861028181374,52.4165984599033,27.9519367227509)) ;
#17328 = CARTESIAN_POINT('Ctrl Pts',(84.1795678229038,51.6408181792509,28.0150644063488)) ;
#17329 = CARTESIAN_POINT('Ctrl Pts',(84.989450350052,51.4618012935295,28.0781920899466)) ;
#17330 = CARTESIAN_POINT('Ctrl Pts',(85.5825562620867,52.0416134444791,28.1413197735445)) ;
#17331 = CARTESIAN_POINT('Ctrl Pts',(85.4219412946177,52.8553453323684,28.2044474571424)) ;
#17332 = CARTESIAN_POINT('Ctrl Pts',(84.6530116623168,53.1663179577801,28.2675751407402)) ;
#17333 = CARTESIAN_POINT('Ctrl Pts',(83.9718864685879,52.693004928524,28.3307028243381)) ;
#17334 = CARTESIAN_POINT('Ctrl Pts',(83.9951946470391,51.8639009048952,28.393830507936)) ;
#17335 = CARTESIAN_POINT('Ctrl Pts',(84.7018350882737,51.4296014229731,28.4569581915339)) ;
#17336 = CARTESIAN_POINT('Ctrl Pts',(85.4520796692884,51.7832818180256,28.5200858751317)) ;
#17337 = CARTESIAN_POINT('Ctrl Pts',(85.566725036296,52.6047519593021,28.5832135587296)) ;
#17338 = CARTESIAN_POINT('Ctrl Pts',(84.9419816788649,53.1503273349667,28.6463412423274)) ;
#17339 = CARTESIAN_POINT('Ctrl Pts',(84.1434355330495,52.9260935146161,28.7094689259253)) ;
#17340 = CARTESIAN_POINT('Ctrl Pts',(83.8940178057069,52.1350514484319,28.7725966095232)) ;
#17341 = CARTESIAN_POINT('Ctrl Pts',(84.4195286707959,51.4933388306201,28.835724293121)) ;
#17342 = CARTESIAN_POINT('Ctrl Pts',(85.2442182847965,51.5819040255063,28.8988519767189)) ;
#17343 = CARTESIAN_POINT('Ctrl Pts',(85.6214875174565,52.3205681435423,28.9619796603168)) ;
#17344 = CARTESIAN_POINT('Ctrl Pts',(85.2097910453075,53.0406117311157,29.0251073439146)) ;
#17345 = CARTESIAN_POINT('Ctrl Pts',(84.3818414899421,53.090172672954,29.0882350275125)) ;
#17346 = CARTESIAN_POINT('Ctrl Pts',(83.887189236662,52.4243829903134,29.1513627111104)) ;
#17347 = CARTESIAN_POINT('Ctrl Pts',(84.1736475424871,51.6459882368565,29.2144903947082)) ;
#17348 = CARTESIAN_POINT('Ctrl Pts',(84.9818830553883,51.4596763776764,29.2776180783061)) ;
#17349 = CARTESIAN_POINT('Ctrl Pts',(85.5801926949256,52.0341172609902,29.340745761904)) ;
#17350 = CARTESIAN_POINT('Ctrl Pts',(85.4269212141838,52.8492642455131,29.4038734455019)) ;
#17351 = CARTESIAN_POINT('Ctrl Pts',(84.6608267013838,53.1671572316628,29.4670011290997)) ;
#17352 = CARTESIAN_POINT('Ctrl Pts',(83.9754616000595,52.7000047607579,29.5301288126976)) ;
#17353 = CARTESIAN_POINT('Ctrl Pts',(83.9912932713457,51.8707242826505,29.5932564962954)) ;
#17354 = CARTESIAN_POINT('Ctrl Pts',(84.6939891568927,51.4300710793027,29.6563841798933)) ;
#17355 = CARTESIAN_POINT('Ctrl Pts',(85.4473921764194,51.7769725687113,29.7195118634912)) ;
#17356 = CARTESIAN_POINT('Ctrl Pts',(85.5694396125602,52.5973756260661,29.7826395470891)) ;
#17357 = CARTESIAN_POINT('Ctrl Pts',(84.9496407932796,53.1485617804674,29.8457672306869)) ;
#17358 = CARTESIAN_POINT('Ctrl Pts',(84.1491053185406,52.9315371116611,29.9088949142848)) ;
#17359 = CARTESIAN_POINT('Ctrl Pts',(83.8925653530632,52.1427760583006,29.9720225978826)) ;
#17360 = CARTESIAN_POINT('Ctrl Pts',(84.4122688988207,51.4963512925987,30.0351502814805)) ;
#17361 = CARTESIAN_POINT('Ctrl Pts',(85.237723532162,51.5774771299215,30.0982779650784)) ;
#17362 = CARTESIAN_POINT('Ctrl Pts',(85.6216375437542,52.3127095998846,30.1614056486762)) ;
#17363 = CARTESIAN_POINT('Ctrl Pts',(85.2164500303437,53.036435951597,30.2245333322741)) ;
#17364 = CARTESIAN_POINT('Ctrl Pts',(84.3889809930133,53.0934600293675,30.2876610158719)) ;
#17365 = CARTESIAN_POINT('Ctrl Pts',(83.8883457996475,52.4321574085169,30.3507886994698)) ;
#17366 = CARTESIAN_POINT('Ctrl Pts',(84.167774118224,51.6512114641819,30.4139163830677)) ;
#17367 = CARTESIAN_POINT('Ctrl Pts',(84.9742969091548,51.4576197781646,30.4770440666656)) ;
#17368 = CARTESIAN_POINT('Ctrl Pts',(85.5777616350177,52.0266426931532,30.5401717502634)) ;
#17369 = CARTESIAN_POINT('Ctrl Pts',(85.4318461016247,52.8431385047737,30.6032994338613)) ;
#17370 = CARTESIAN_POINT('Ctrl Pts',(84.6686489900153,53.1679260075878,30.6664271174592)) ;
#17371 = CARTESIAN_POINT('Ctrl Pts',(83.9790996997554,52.7069720736917,30.729554801057)) ;
#17372 = CARTESIAN_POINT('Ctrl Pts',(83.9874535766736,51.8775825591953,30.7926824846549)) ;
#17373 = CARTESIAN_POINT('Ctrl Pts',(84.6861477792349,51.4306114595269,30.8558101682528)) ;
#17374 = CARTESIAN_POINT('Ctrl Pts',(85.4426479868293,51.7707058389346,30.9189378518506)) ;
#17375 = CARTESIAN_POINT('Ctrl Pts',(85.5720875709808,52.5899751196893,30.9820655354485)) ;
#17376 = CARTESIAN_POINT('Ctrl Pts',(84.9572836759283,53.14672723415,31.0451932190464)) ;
#17377 = CARTESIAN_POINT('Ctrl Pts',(84.1548239582845,52.9369293777739,31.1083209026442)) ;
#17378 = CARTESIAN_POINT('Ctrl Pts',(83.8911826019863,52.1505134266192,31.1714485862421)) ;
#17379 = CARTESIAN_POINT('Ctrl Pts',(84.4050365955573,51.4994291370381,31.2345762698399)) ;
#17380 = CARTESIAN_POINT('Ctrl Pts',(85.2311891044738,51.5731088770259,31.2977039534378)) ;
#17381 = CARTESIAN_POINT('Ctrl Pts',(85.6217167571572,52.3048502193085,31.3608316370357)) ;
#17382 = CARTESIAN_POINT('Ctrl Pts',(85.2230709941749,53.0321999030888,31.4239593206336)) ;
#17383 = CARTESIAN_POINT('Ctrl Pts',(84.3961500488167,53.0966836878991,31.4870870042314)) ;
#17384 = CARTESIAN_POINT('Ctrl Pts',(83.8895720017401,52.439919441728,31.5502146878293)) ;
#17385 = CARTESIAN_POINT('Ctrl Pts',(84.1619488624328,51.6564907664694,31.6133423714271)) ;
#17386 = CARTESIAN_POINT('Ctrl Pts',(84.9666908338978,51.4556249045992,31.676470055025)) ;
#17387 = CARTESIAN_POINT('Ctrl Pts',(85.5752667181236,52.0192040621772,31.7395977386228)) ;
#17388 = CARTESIAN_POINT('Ctrl Pts',(85.4367085793821,52.836940778588,31.8027254222208)) ;
#17389 = CARTESIAN_POINT('Ctrl Pts',(84.6764920518234,53.1686806993748,31.8658531058186)) ;
#17390 = CARTESIAN_POINT('Ctrl Pts',(83.9827717291772,52.7137916825236,31.9289807894165)) ;
#17391 = CARTESIAN_POINT('Ctrl Pts',(83.9837342921951,51.8847078895634,31.9921084730144)) ;
#17392 = CARTESIAN_POINT('Ctrl Pts',(84.6781907808013,51.4307481373616,32.0552361566122)) ;
#17393 = CARTESIAN_POINT('Ctrl Pts',(85.4381029288359,51.7654662125157,32.1183638402101)) ;
#17394 = CARTESIAN_POINT('Ctrl Pts',(85.5282772224873,52.308450710684,32.1604489626087)) ;
#17395 = CARTESIAN_POINT('Ctrl Pts',(85.4491041092583,52.5395296316078,32.181491523808)) ;
#17396 = CARTESIAN_POINT('Ctrl Pts',(85.6645587247977,52.6133494876276,32.05)) ;
#17397 = CARTESIAN_POINT('Ctrl Pts',(85.7681319415962,52.3110551076505,32.0289574388007)) ;
#17398 = CARTESIAN_POINT('Ctrl Pts',(85.7091495340268,51.9558925477018,32.0079148776014)) ;
#17399 = CARTESIAN_POINT('Ctrl Pts',(85.5139738311189,51.7053323098666,31.9868723164021)) ;
#17400 = CARTESIAN_POINT('Ctrl Pts',(85.318798128211,51.4547720720313,31.9658297552029)) ;
#17401 = CARTESIAN_POINT('Ctrl Pts',(84.9874291299646,51.3088141563095,31.9447871940036)) ;
#17402 = CARTESIAN_POINT('Ctrl Pts',(84.6703315026591,51.3348125530812,31.9237446328043)) ;
#17403 = CARTESIAN_POINT('Ctrl Pts',(84.3532338753536,51.360810949853,31.902702071605)) ;
#17404 = CARTESIAN_POINT('Ctrl Pts',(84.0504076189891,51.5587656591183,31.8816595104057)) ;
#17405 = CARTESIAN_POINT('Ctrl Pts',(83.898784622111,51.8385090843067,31.8606169492064)) ;
#17406 = CARTESIAN_POINT('Ctrl Pts',(83.8228117423715,51.9786785443315,31.8500732717675)) ;
#17407 = CARTESIAN_POINT('Ctrl Pts',(83.7848007833449,52.1393823285476,31.8395295943286)) ;
#17408 = CARTESIAN_POINT('Ctrl Pts',(83.7847843561952,52.3000678891362,31.8289859168897)) ;
#17409 = CARTESIAN_POINT('Origin',(84.75,52.3,26.5)) ;
#17410 = CARTESIAN_POINT('',(85.81675,52.3,26.4)) ;
#17411 = CARTESIAN_POINT('Origin',(85.81675,52.3,26.5)) ;
#17412 = CARTESIAN_POINT('Origin',(84.75,52.3,26.4)) ;
#17413 = CARTESIAN_POINT('Origin',(84.75,52.3,26.4)) ;
#17414 = CARTESIAN_POINT('Origin',(84.75,52.3,32.05)) ;
#17415 = CARTESIAN_POINT('Origin',(84.75,52.3,26.4)) ;
#17416 = CARTESIAN_POINT('',(83.05,52.3,26.4)) ;
#17417 = CARTESIAN_POINT('Origin',(84.75,52.3,26.4)) ;
#17418 = CARTESIAN_POINT('Origin',(84.75,52.3,32.225)) ;
#17419 = CARTESIAN_POINT('',(84.13325,52.3,32.4)) ;
#17420 = CARTESIAN_POINT('',(83.95825,52.3,32.225)) ;
#17421 = CARTESIAN_POINT('Origin',(84.75,52.3,32.4)) ;
#17422 = CARTESIAN_POINT('Origin',(84.75,52.3,32.4)) ;
#17423 = CARTESIAN_POINT('Origin',(86.6949953121991,51.9570448491078,25.8)) ;
#17424 = CARTESIAN_POINT('',(86.6111892234686,51.9179336779508,25.8)) ;
#17425 = CARTESIAN_POINT('',(86.6296201574069,52.0224606985135,25.8)) ;
#17426 = CARTESIAN_POINT('Origin',(84.75,52.3,25.8)) ;
#17427 = CARTESIAN_POINT('',(86.4734135677714,51.9961156890829,25.8)) ;
#17428 = CARTESIAN_POINT('',(86.4734135677714,51.9961156890829,25.8)) ;
#17429 = CARTESIAN_POINT('',(86.9443607650536,52.0755432496147,25.8)) ;
#17430 = CARTESIAN_POINT('Origin',(86.9443607650536,52.0755432496147,24.4)) ;
#17431 = CARTESIAN_POINT('',(86.6296201574069,52.0224606985135,24.7)) ;
#17432 = CARTESIAN_POINT('',(86.6296201574069,52.0224606985135,26.4)) ;
#17433 = CARTESIAN_POINT('',(86.4734135677714,51.9961156890829,24.55)) ;
#17434 = CARTESIAN_POINT('',(86.4734135677714,51.9961156890829,24.4)) ;
#17435 = CARTESIAN_POINT('Ctrl Pts',(86.6296201574069,52.0224606985136,24.7)) ;
#17436 = CARTESIAN_POINT('Ctrl Pts',(86.5483071381441,52.0087468579879,24.6215623892917)) ;
#17437 = CARTESIAN_POINT('Ctrl Pts',(86.4734135677714,51.9961156890829,24.55)) ;
#17438 = CARTESIAN_POINT('Origin',(86.4734135677714,51.9961156890829,24.4)) ;
#17439 = CARTESIAN_POINT('',(86.6111892234686,51.9179336779508,24.7)) ;
#17440 = CARTESIAN_POINT('',(86.6111892234686,51.9179336779508,26.4)) ;
#17441 = CARTESIAN_POINT('Ctrl Pts',(86.4734135677714,51.9961156890829,24.55)) ;
#17442 = CARTESIAN_POINT('Ctrl Pts',(86.539470388997,51.9586311631971,24.6215623892931)) ;
#17443 = CARTESIAN_POINT('Ctrl Pts',(86.6111892234686,51.9179336779507,24.7)) ;
#17444 = CARTESIAN_POINT('Origin',(84.75,52.3,26.4)) ;
#17445 = CARTESIAN_POINT('',(86.6492586976664,52.2469302408297,24.7)) ;
#17446 = CARTESIAN_POINT('Origin',(84.75,52.3,24.7)) ;
#17447 = CARTESIAN_POINT('',(86.6492586976664,52.2469302408297,25.8)) ;
#17448 = CARTESIAN_POINT('',(86.6492586976664,52.2469302408297,26.4)) ;
#17449 = CARTESIAN_POINT('',(86.6492586976664,52.3530697591703,25.8)) ;
#17450 = CARTESIAN_POINT('Origin',(84.75,52.3,25.8)) ;
#17451 = CARTESIAN_POINT('',(86.6492586976664,52.3530697591703,24.7)) ;
#17452 = CARTESIAN_POINT('',(86.6492586976664,52.3530697591703,26.4)) ;
#17453 = CARTESIAN_POINT('',(86.6296201574069,52.5775393014865,24.7)) ;
#17454 = CARTESIAN_POINT('Origin',(84.75,52.3,24.7)) ;
#17455 = CARTESIAN_POINT('',(86.6296201574069,52.5775393014865,25.8)) ;
#17456 = CARTESIAN_POINT('',(86.6296201574069,52.5775393014865,26.4)) ;
#17457 = CARTESIAN_POINT('',(86.6111892234686,52.6820663220492,25.8)) ;
#17458 = CARTESIAN_POINT('Origin',(84.75,52.3,25.8)) ;
#17459 = CARTESIAN_POINT('',(86.6111892234686,52.6820663220492,24.7)) ;
#17460 = CARTESIAN_POINT('',(86.6111892234686,52.6820663220492,26.4)) ;
#17461 = CARTESIAN_POINT('',(86.5528703097983,52.8997154709092,24.7)) ;
#17462 = CARTESIAN_POINT('Origin',(84.75,52.3,24.7)) ;
#17463 = CARTESIAN_POINT('',(86.5528703097983,52.8997154709092,25.8)) ;
#17464 = CARTESIAN_POINT('',(86.5528703097983,52.8997154709092,26.4)) ;
#17465 = CARTESIAN_POINT('',(86.5165684565229,52.9994539930676,25.8)) ;
#17466 = CARTESIAN_POINT('Origin',(84.75,52.3,25.8)) ;
#17467 = CARTESIAN_POINT('',(86.5165684565229,52.9994539930676,24.7)) ;
#17468 = CARTESIAN_POINT('',(86.5165684565229,52.9994539930676,26.4)) ;
#17469 = CARTESIAN_POINT('',(86.4213411601228,53.203669589219,24.7)) ;
#17470 = CARTESIAN_POINT('Origin',(84.75,52.3,24.7)) ;
#17471 = CARTESIAN_POINT('',(86.4213411601228,53.203669589219,25.8)) ;
#17472 = CARTESIAN_POINT('',(86.4213411601228,53.203669589219,26.4)) ;
#17473 = CARTESIAN_POINT('',(86.3682714009525,53.2955891084474,25.8)) ;
#17474 = CARTESIAN_POINT('Origin',(84.75,52.3,25.8)) ;
#17475 = CARTESIAN_POINT('',(86.3682714009525,53.2955891084474,24.7)) ;
#17476 = CARTESIAN_POINT('',(86.3682714009525,53.2955891084474,26.4)) ;
#17477 = CARTESIAN_POINT('',(86.2390291550365,53.4801661643393,24.7)) ;
#17478 = CARTESIAN_POINT('Origin',(84.75,52.3,24.7)) ;
#17479 = CARTESIAN_POINT('',(86.2390291550365,53.4801661643393,25.8)) ;
#17480 = CARTESIAN_POINT('',(86.2390291550365,53.4801661643393,26.4)) ;
#17481 = CARTESIAN_POINT('',(86.170803987749,53.5614737525594,25.8)) ;
#17482 = CARTESIAN_POINT('Origin',(84.75,52.3,25.8)) ;
#17483 = CARTESIAN_POINT('',(86.170803987749,53.5614737525594,24.7)) ;
#17484 = CARTESIAN_POINT('',(86.170803987749,53.5614737525594,26.4)) ;
#17485 = CARTESIAN_POINT('',(86.0114737525594,53.7208039877491,24.7)) ;
#17486 = CARTESIAN_POINT('Origin',(84.75,52.3,24.7)) ;
#17487 = CARTESIAN_POINT('',(86.0114737525594,53.7208039877491,25.8)) ;
#17488 = CARTESIAN_POINT('',(86.0114737525594,53.7208039877491,26.4)) ;
#17489 = CARTESIAN_POINT('',(85.9301661643393,53.7890291550365,25.8)) ;
#17490 = CARTESIAN_POINT('Origin',(84.75,52.3,25.8)) ;
#17491 = CARTESIAN_POINT('',(85.9301661643393,53.7890291550365,24.7)) ;
#17492 = CARTESIAN_POINT('',(85.9301661643393,53.7890291550365,26.4)) ;
#17493 = CARTESIAN_POINT('',(85.7455891084474,53.9182714009525,24.7)) ;
#17494 = CARTESIAN_POINT('Origin',(84.75,52.3,24.7)) ;
#17495 = CARTESIAN_POINT('',(85.7455891084474,53.9182714009525,25.8)) ;
#17496 = CARTESIAN_POINT('',(85.7455891084474,53.9182714009525,26.4)) ;
#17497 = CARTESIAN_POINT('',(85.653669589219,53.9713411601228,25.8)) ;
#17498 = CARTESIAN_POINT('Origin',(84.75,52.3,25.8)) ;
#17499 = CARTESIAN_POINT('',(85.653669589219,53.9713411601228,24.7)) ;
#17500 = CARTESIAN_POINT('',(85.653669589219,53.9713411601228,26.4)) ;
#17501 = CARTESIAN_POINT('',(85.4494539930676,54.0665684565229,24.7)) ;
#17502 = CARTESIAN_POINT('Origin',(84.75,52.3,24.7)) ;
#17503 = CARTESIAN_POINT('',(85.4494539930676,54.0665684565229,25.8)) ;
#17504 = CARTESIAN_POINT('',(85.4494539930676,54.0665684565229,26.4)) ;
#17505 = CARTESIAN_POINT('',(85.3497154709092,54.1028703097983,25.8)) ;
#17506 = CARTESIAN_POINT('Origin',(84.75,52.3,25.8)) ;
#17507 = CARTESIAN_POINT('',(85.3497154709092,54.1028703097983,24.7)) ;
#17508 = CARTESIAN_POINT('',(85.3497154709092,54.1028703097983,26.4)) ;
#17509 = CARTESIAN_POINT('',(85.1320663220492,54.1611892234686,24.7)) ;
#17510 = CARTESIAN_POINT('Origin',(84.75,52.3,24.7)) ;
#17511 = CARTESIAN_POINT('',(85.1320663220492,54.1611892234686,25.8)) ;
#17512 = CARTESIAN_POINT('',(85.1320663220492,54.1611892234686,26.4)) ;
#17513 = CARTESIAN_POINT('',(85.0275393014864,54.1796201574069,25.8)) ;
#17514 = CARTESIAN_POINT('Origin',(84.75,52.3,25.8)) ;
#17515 = CARTESIAN_POINT('',(85.0275393014864,54.1796201574069,24.7)) ;
#17516 = CARTESIAN_POINT('',(85.0275393014864,54.1796201574069,26.4)) ;
#17517 = CARTESIAN_POINT('',(84.8030697591703,54.1992586976664,24.7)) ;
#17518 = CARTESIAN_POINT('Origin',(84.75,52.3,24.7)) ;
#17519 = CARTESIAN_POINT('',(84.8030697591703,54.1992586976664,25.8)) ;
#17520 = CARTESIAN_POINT('',(84.8030697591703,54.1992586976664,26.4)) ;
#17521 = CARTESIAN_POINT('',(84.6969302408297,54.1992586976664,25.8)) ;
#17522 = CARTESIAN_POINT('Origin',(84.75,52.3,25.8)) ;
#17523 = CARTESIAN_POINT('',(84.6969302408297,54.1992586976664,24.7)) ;
#17524 = CARTESIAN_POINT('',(84.6969302408297,54.1992586976664,26.4)) ;
#17525 = CARTESIAN_POINT('',(84.4724606985135,54.1796201574069,24.7)) ;
#17526 = CARTESIAN_POINT('Origin',(84.75,52.3,24.7)) ;
#17527 = CARTESIAN_POINT('',(84.4724606985135,54.1796201574069,25.8)) ;
#17528 = CARTESIAN_POINT('',(84.4724606985135,54.1796201574069,26.4)) ;
#17529 = CARTESIAN_POINT('',(84.3679336779508,54.1611892234686,25.8)) ;
#17530 = CARTESIAN_POINT('Origin',(84.75,52.3,25.8)) ;
#17531 = CARTESIAN_POINT('',(84.3679336779508,54.1611892234686,24.7)) ;
#17532 = CARTESIAN_POINT('',(84.3679336779508,54.1611892234686,26.4)) ;
#17533 = CARTESIAN_POINT('',(84.1502845290908,54.1028703097983,24.7)) ;
#17534 = CARTESIAN_POINT('Origin',(84.75,52.3,24.7)) ;
#17535 = CARTESIAN_POINT('',(84.1502845290908,54.1028703097983,25.8)) ;
#17536 = CARTESIAN_POINT('',(84.1502845290908,54.1028703097983,26.4)) ;
#17537 = CARTESIAN_POINT('',(84.0505460069324,54.0665684565229,25.8)) ;
#17538 = CARTESIAN_POINT('Origin',(84.75,52.3,25.8)) ;
#17539 = CARTESIAN_POINT('',(84.0505460069324,54.0665684565229,24.7)) ;
#17540 = CARTESIAN_POINT('',(84.0505460069324,54.0665684565229,26.4)) ;
#17541 = CARTESIAN_POINT('',(83.8463304107809,53.9713411601228,24.7)) ;
#17542 = CARTESIAN_POINT('Origin',(84.75,52.3,24.7)) ;
#17543 = CARTESIAN_POINT('',(83.8463304107809,53.9713411601228,25.8)) ;
#17544 = CARTESIAN_POINT('',(83.8463304107809,53.9713411601228,26.4)) ;
#17545 = CARTESIAN_POINT('',(83.7544108915526,53.9182714009525,25.8)) ;
#17546 = CARTESIAN_POINT('Origin',(84.75,52.3,25.8)) ;
#17547 = CARTESIAN_POINT('',(83.7544108915526,53.9182714009525,24.7)) ;
#17548 = CARTESIAN_POINT('',(83.7544108915526,53.9182714009525,26.4)) ;
#17549 = CARTESIAN_POINT('',(83.5698338356607,53.7890291550365,24.7)) ;
#17550 = CARTESIAN_POINT('Origin',(84.75,52.3,24.7)) ;
#17551 = CARTESIAN_POINT('',(83.5698338356607,53.7890291550365,25.8)) ;
#17552 = CARTESIAN_POINT('',(83.5698338356607,53.7890291550365,26.4)) ;
#17553 = CARTESIAN_POINT('',(83.4885262474406,53.7208039877491,25.8)) ;
#17554 = CARTESIAN_POINT('Origin',(84.75,52.3,25.8)) ;
#17555 = CARTESIAN_POINT('',(83.4885262474406,53.7208039877491,24.7)) ;
#17556 = CARTESIAN_POINT('',(83.4885262474406,53.7208039877491,26.4)) ;
#17557 = CARTESIAN_POINT('',(83.3291960122509,53.5614737525594,24.7)) ;
#17558 = CARTESIAN_POINT('Origin',(84.75,52.3,24.7)) ;
#17559 = CARTESIAN_POINT('',(83.3291960122509,53.5614737525594,25.8)) ;
#17560 = CARTESIAN_POINT('',(83.3291960122509,53.5614737525594,26.4)) ;
#17561 = CARTESIAN_POINT('',(83.2609708449635,53.4801661643393,25.8)) ;
#17562 = CARTESIAN_POINT('Origin',(84.75,52.3,25.8)) ;
#17563 = CARTESIAN_POINT('',(83.2609708449635,53.4801661643393,24.7)) ;
#17564 = CARTESIAN_POINT('',(83.2609708449635,53.4801661643393,26.4)) ;
#17565 = CARTESIAN_POINT('',(83.1317285990475,53.2955891084474,24.7)) ;
#17566 = CARTESIAN_POINT('Origin',(84.75,52.3,24.7)) ;
#17567 = CARTESIAN_POINT('',(83.1317285990475,53.2955891084474,25.8)) ;
#17568 = CARTESIAN_POINT('',(83.1317285990475,53.2955891084474,26.4)) ;
#17569 = CARTESIAN_POINT('',(83.0786588398772,53.203669589219,25.8)) ;
#17570 = CARTESIAN_POINT('Origin',(84.75,52.3,25.8)) ;
#17571 = CARTESIAN_POINT('',(83.0786588398772,53.203669589219,24.7)) ;
#17572 = CARTESIAN_POINT('',(83.0786588398772,53.203669589219,26.4)) ;
#17573 = CARTESIAN_POINT('',(82.9834315434771,52.9994539930676,24.7)) ;
#17574 = CARTESIAN_POINT('Origin',(84.75,52.3,24.7)) ;
#17575 = CARTESIAN_POINT('',(82.9834315434771,52.9994539930676,25.8)) ;
#17576 = CARTESIAN_POINT('',(82.9834315434771,52.9994539930676,26.4)) ;
#17577 = CARTESIAN_POINT('',(82.9471296902017,52.8997154709092,25.8)) ;
#17578 = CARTESIAN_POINT('Origin',(84.75,52.3,25.8)) ;
#17579 = CARTESIAN_POINT('',(82.9471296902017,52.8997154709092,24.7)) ;
#17580 = CARTESIAN_POINT('',(82.9471296902017,52.8997154709092,26.4)) ;
#17581 = CARTESIAN_POINT('',(82.8888107765314,52.6820663220492,24.7)) ;
#17582 = CARTESIAN_POINT('Origin',(84.75,52.3,24.7)) ;
#17583 = CARTESIAN_POINT('',(82.8888107765314,52.6820663220492,25.8)) ;
#17584 = CARTESIAN_POINT('',(82.8888107765314,52.6820663220492,26.4)) ;
#17585 = CARTESIAN_POINT('',(82.8703798425931,52.5775393014865,25.8)) ;
#17586 = CARTESIAN_POINT('Origin',(84.75,52.3,25.8)) ;
#17587 = CARTESIAN_POINT('',(82.8703798425931,52.5775393014865,24.7)) ;
#17588 = CARTESIAN_POINT('',(82.8703798425931,52.5775393014865,26.4)) ;
#17589 = CARTESIAN_POINT('',(82.8507413023336,52.3530697591703,24.7)) ;
#17590 = CARTESIAN_POINT('Origin',(84.75,52.3,24.7)) ;
#17591 = CARTESIAN_POINT('',(82.8507413023336,52.3530697591703,25.8)) ;
#17592 = CARTESIAN_POINT('',(82.8507413023336,52.3530697591703,26.4)) ;
#17593 = CARTESIAN_POINT('',(82.85,52.3,25.8)) ;
#17594 = CARTESIAN_POINT('Origin',(84.75,52.3,25.8)) ;
#17595 = CARTESIAN_POINT('',(82.85,52.3,26.2)) ;
#17596 = CARTESIAN_POINT('',(82.85,52.3,26.4)) ;
#17597 = CARTESIAN_POINT('Origin',(84.75,52.3,26.2)) ;
#17598 = CARTESIAN_POINT('',(82.8507413023336,52.2469302408297,25.8)) ;
#17599 = CARTESIAN_POINT('Origin',(84.75,52.3,25.8)) ;
#17600 = CARTESIAN_POINT('',(82.8507413023336,52.2469302408297,24.7)) ;
#17601 = CARTESIAN_POINT('',(82.8507413023336,52.2469302408297,26.4)) ;
#17602 = CARTESIAN_POINT('',(82.8703798425931,52.0224606985135,24.7)) ;
#17603 = CARTESIAN_POINT('Origin',(84.75,52.3,24.7)) ;
#17604 = CARTESIAN_POINT('',(82.8703798425931,52.0224606985135,25.8)) ;
#17605 = CARTESIAN_POINT('',(82.8703798425931,52.0224606985135,26.4)) ;
#17606 = CARTESIAN_POINT('',(82.8888107765314,51.9179336779508,25.8)) ;
#17607 = CARTESIAN_POINT('Origin',(84.75,52.3,25.8)) ;
#17608 = CARTESIAN_POINT('',(82.8888107765314,51.9179336779508,24.7)) ;
#17609 = CARTESIAN_POINT('',(82.8888107765314,51.9179336779508,26.4)) ;
#17610 = CARTESIAN_POINT('',(82.9471296902017,51.7002845290908,24.7)) ;
#17611 = CARTESIAN_POINT('Origin',(84.75,52.3,24.7)) ;
#17612 = CARTESIAN_POINT('',(82.9471296902017,51.7002845290908,25.8)) ;
#17613 = CARTESIAN_POINT('',(82.9471296902017,51.7002845290908,26.4)) ;
#17614 = CARTESIAN_POINT('',(82.9834315434771,51.6005460069324,25.8)) ;
#17615 = CARTESIAN_POINT('Origin',(84.75,52.3,25.8)) ;
#17616 = CARTESIAN_POINT('',(82.9834315434771,51.6005460069324,24.7)) ;
#17617 = CARTESIAN_POINT('',(82.9834315434771,51.6005460069324,26.4)) ;
#17618 = CARTESIAN_POINT('',(83.0786588398772,51.396330410781,24.7)) ;
#17619 = CARTESIAN_POINT('Origin',(84.75,52.3,24.7)) ;
#17620 = CARTESIAN_POINT('',(83.0786588398772,51.396330410781,25.8)) ;
#17621 = CARTESIAN_POINT('',(83.0786588398772,51.396330410781,26.4)) ;
#17622 = CARTESIAN_POINT('',(83.1317285990474,51.3044108915526,25.8)) ;
#17623 = CARTESIAN_POINT('Origin',(84.75,52.3,25.8)) ;
#17624 = CARTESIAN_POINT('',(83.1317285990474,51.3044108915526,24.7)) ;
#17625 = CARTESIAN_POINT('',(83.1317285990474,51.3044108915526,26.4)) ;
#17626 = CARTESIAN_POINT('',(83.2609708449635,51.1198338356607,24.7)) ;
#17627 = CARTESIAN_POINT('Origin',(84.75,52.3,24.7)) ;
#17628 = CARTESIAN_POINT('',(83.2609708449635,51.1198338356607,25.8)) ;
#17629 = CARTESIAN_POINT('',(83.2609708449635,51.1198338356607,26.4)) ;
#17630 = CARTESIAN_POINT('',(83.3291960122509,51.0385262474406,25.8)) ;
#17631 = CARTESIAN_POINT('Origin',(84.75,52.3,25.8)) ;
#17632 = CARTESIAN_POINT('',(83.3291960122509,51.0385262474406,24.7)) ;
#17633 = CARTESIAN_POINT('',(83.3291960122509,51.0385262474406,26.4)) ;
#17634 = CARTESIAN_POINT('',(83.4885262474406,50.8791960122509,24.7)) ;
#17635 = CARTESIAN_POINT('Origin',(84.75,52.3,24.7)) ;
#17636 = CARTESIAN_POINT('',(83.4885262474406,50.8791960122509,25.8)) ;
#17637 = CARTESIAN_POINT('',(83.4885262474406,50.8791960122509,26.4)) ;
#17638 = CARTESIAN_POINT('',(83.5698338356607,50.8109708449635,25.8)) ;
#17639 = CARTESIAN_POINT('Origin',(84.75,52.3,25.8)) ;
#17640 = CARTESIAN_POINT('',(83.5698338356607,50.8109708449635,24.7)) ;
#17641 = CARTESIAN_POINT('',(83.5698338356607,50.8109708449635,26.4)) ;
#17642 = CARTESIAN_POINT('',(83.7544108915526,50.6817285990475,24.7)) ;
#17643 = CARTESIAN_POINT('Origin',(84.75,52.3,24.7)) ;
#17644 = CARTESIAN_POINT('',(83.7544108915526,50.6817285990475,25.8)) ;
#17645 = CARTESIAN_POINT('',(83.7544108915526,50.6817285990475,26.4)) ;
#17646 = CARTESIAN_POINT('',(83.846330410781,50.6286588398772,25.8)) ;
#17647 = CARTESIAN_POINT('Origin',(84.75,52.3,25.8)) ;
#17648 = CARTESIAN_POINT('',(83.846330410781,50.6286588398772,24.7)) ;
#17649 = CARTESIAN_POINT('',(83.846330410781,50.6286588398772,26.4)) ;
#17650 = CARTESIAN_POINT('',(84.0505460069324,50.5334315434771,24.7)) ;
#17651 = CARTESIAN_POINT('Origin',(84.75,52.3,24.7)) ;
#17652 = CARTESIAN_POINT('',(84.0505460069324,50.5334315434771,25.8)) ;
#17653 = CARTESIAN_POINT('',(84.0505460069324,50.5334315434771,26.4)) ;
#17654 = CARTESIAN_POINT('',(84.1502845290908,50.4971296902017,25.8)) ;
#17655 = CARTESIAN_POINT('Origin',(84.75,52.3,25.8)) ;
#17656 = CARTESIAN_POINT('',(84.1502845290908,50.4971296902017,24.7)) ;
#17657 = CARTESIAN_POINT('',(84.1502845290908,50.4971296902017,26.4)) ;
#17658 = CARTESIAN_POINT('',(84.3679336779508,50.4388107765314,24.7)) ;
#17659 = CARTESIAN_POINT('Origin',(84.75,52.3,24.7)) ;
#17660 = CARTESIAN_POINT('',(84.3679336779508,50.4388107765314,25.8)) ;
#17661 = CARTESIAN_POINT('',(84.3679336779508,50.4388107765314,26.4)) ;
#17662 = CARTESIAN_POINT('',(84.4724606985135,50.4203798425931,25.8)) ;
#17663 = CARTESIAN_POINT('Origin',(84.75,52.3,25.8)) ;
#17664 = CARTESIAN_POINT('',(84.4724606985135,50.4203798425931,24.7)) ;
#17665 = CARTESIAN_POINT('',(84.4724606985135,50.4203798425931,26.4)) ;
#17666 = CARTESIAN_POINT('',(84.6969302408297,50.4007413023336,24.7)) ;
#17667 = CARTESIAN_POINT('Origin',(84.75,52.3,24.7)) ;
#17668 = CARTESIAN_POINT('',(84.6969302408297,50.4007413023336,25.8)) ;
#17669 = CARTESIAN_POINT('',(84.6969302408297,50.4007413023336,26.4)) ;
#17670 = CARTESIAN_POINT('',(84.8030697591703,50.4007413023336,25.8)) ;
#17671 = CARTESIAN_POINT('Origin',(84.75,52.3,25.8)) ;
#17672 = CARTESIAN_POINT('',(84.8030697591703,50.4007413023336,24.7)) ;
#17673 = CARTESIAN_POINT('',(84.8030697591703,50.4007413023336,26.4)) ;
#17674 = CARTESIAN_POINT('',(85.0275393014864,50.4203798425931,24.7)) ;
#17675 = CARTESIAN_POINT('Origin',(84.75,52.3,24.7)) ;
#17676 = CARTESIAN_POINT('',(85.0275393014864,50.4203798425931,25.8)) ;
#17677 = CARTESIAN_POINT('',(85.0275393014864,50.4203798425931,26.4)) ;
#17678 = CARTESIAN_POINT('',(85.1320663220492,50.4388107765314,25.8)) ;
#17679 = CARTESIAN_POINT('Origin',(84.75,52.3,25.8)) ;
#17680 = CARTESIAN_POINT('',(85.1320663220492,50.4388107765314,24.7)) ;
#17681 = CARTESIAN_POINT('',(85.1320663220492,50.4388107765314,26.4)) ;
#17682 = CARTESIAN_POINT('',(85.3497154709092,50.4971296902017,24.7)) ;
#17683 = CARTESIAN_POINT('Origin',(84.75,52.3,24.7)) ;
#17684 = CARTESIAN_POINT('',(85.3497154709092,50.4971296902017,25.8)) ;
#17685 = CARTESIAN_POINT('',(85.3497154709092,50.4971296902017,26.4)) ;
#17686 = CARTESIAN_POINT('',(85.4494539930676,50.5334315434771,25.8)) ;
#17687 = CARTESIAN_POINT('Origin',(84.75,52.3,25.8)) ;
#17688 = CARTESIAN_POINT('',(85.4494539930676,50.5334315434771,24.7)) ;
#17689 = CARTESIAN_POINT('',(85.4494539930676,50.5334315434771,26.4)) ;
#17690 = CARTESIAN_POINT('',(85.653669589219,50.6286588398772,24.7)) ;
#17691 = CARTESIAN_POINT('Origin',(84.75,52.3,24.7)) ;
#17692 = CARTESIAN_POINT('',(85.653669589219,50.6286588398772,25.8)) ;
#17693 = CARTESIAN_POINT('',(85.653669589219,50.6286588398772,26.4)) ;
#17694 = CARTESIAN_POINT('',(85.7455891084474,50.6817285990475,25.8)) ;
#17695 = CARTESIAN_POINT('Origin',(84.75,52.3,25.8)) ;
#17696 = CARTESIAN_POINT('',(85.7455891084474,50.6817285990475,24.7)) ;
#17697 = CARTESIAN_POINT('',(85.7455891084474,50.6817285990475,26.4)) ;
#17698 = CARTESIAN_POINT('',(85.9301661643393,50.8109708449635,24.7)) ;
#17699 = CARTESIAN_POINT('Origin',(84.75,52.3,24.7)) ;
#17700 = CARTESIAN_POINT('',(85.9301661643393,50.8109708449635,25.8)) ;
#17701 = CARTESIAN_POINT('',(85.9301661643393,50.8109708449635,26.4)) ;
#17702 = CARTESIAN_POINT('',(86.0114737525594,50.879196012251,25.8)) ;
#17703 = CARTESIAN_POINT('Origin',(84.75,52.3,25.8)) ;
#17704 = CARTESIAN_POINT('',(86.0114737525594,50.879196012251,24.7)) ;
#17705 = CARTESIAN_POINT('',(86.0114737525594,50.879196012251,26.4)) ;
#17706 = CARTESIAN_POINT('',(86.170803987749,51.0385262474406,24.7)) ;
#17707 = CARTESIAN_POINT('Origin',(84.75,52.3,24.7)) ;
#17708 = CARTESIAN_POINT('',(86.170803987749,51.0385262474406,25.8)) ;
#17709 = CARTESIAN_POINT('',(86.170803987749,51.0385262474406,26.4)) ;
#17710 = CARTESIAN_POINT('',(86.2390291550365,51.1198338356607,25.8)) ;
#17711 = CARTESIAN_POINT('Origin',(84.75,52.3,25.8)) ;
#17712 = CARTESIAN_POINT('',(86.2390291550365,51.1198338356607,24.7)) ;
#17713 = CARTESIAN_POINT('',(86.2390291550365,51.1198338356607,26.4)) ;
#17714 = CARTESIAN_POINT('',(86.3682714009525,51.3044108915526,24.7)) ;
#17715 = CARTESIAN_POINT('Origin',(84.75,52.3,24.7)) ;
#17716 = CARTESIAN_POINT('',(86.3682714009525,51.3044108915526,25.8)) ;
#17717 = CARTESIAN_POINT('',(86.3682714009525,51.3044108915526,26.4)) ;
#17718 = CARTESIAN_POINT('',(86.4213411601228,51.396330410781,25.8)) ;
#17719 = CARTESIAN_POINT('Origin',(84.75,52.3,25.8)) ;
#17720 = CARTESIAN_POINT('',(86.4213411601228,51.396330410781,24.7)) ;
#17721 = CARTESIAN_POINT('',(86.4213411601228,51.396330410781,26.4)) ;
#17722 = CARTESIAN_POINT('',(86.5165684565229,51.6005460069324,24.7)) ;
#17723 = CARTESIAN_POINT('Origin',(84.75,52.3,24.7)) ;
#17724 = CARTESIAN_POINT('',(86.5165684565229,51.6005460069324,25.8)) ;
#17725 = CARTESIAN_POINT('',(86.5165684565229,51.6005460069324,26.4)) ;
#17726 = CARTESIAN_POINT('',(86.5528703097983,51.7002845290908,25.8)) ;
#17727 = CARTESIAN_POINT('Origin',(84.75,52.3,25.8)) ;
#17728 = CARTESIAN_POINT('',(86.5528703097983,51.7002845290908,24.7)) ;
#17729 = CARTESIAN_POINT('',(86.5528703097983,51.7002845290908,26.4)) ;
#17730 = CARTESIAN_POINT('Origin',(84.75,52.3,24.7)) ;
#17731 = CARTESIAN_POINT('Origin',(86.8720469886611,51.6979065040093,24.4)) ;
#17732 = CARTESIAN_POINT('',(86.3944620863754,51.7014647491801,25.8)) ;
#17733 = CARTESIAN_POINT('',(86.8720469886611,51.6979065040093,25.8)) ;
#17734 = CARTESIAN_POINT('',(86.3944620863754,51.7014647491801,24.55)) ;
#17735 = CARTESIAN_POINT('',(86.3944620863754,51.7014647491801,24.4)) ;
#17736 = CARTESIAN_POINT('Ctrl Pts',(86.5528703097983,51.7002845290908,24.7)) ;
#17737 = CARTESIAN_POINT('Ctrl Pts',(86.4704112345923,51.7008988902332,24.6215623892926)) ;
#17738 = CARTESIAN_POINT('Ctrl Pts',(86.3944620863753,51.7014647491801,24.55)) ;
#17739 = CARTESIAN_POINT('Origin',(86.3944620863754,51.7014647491801,24.4)) ;
#17740 = CARTESIAN_POINT('Ctrl Pts',(86.3944620863754,51.7014647491801,24.55)) ;
#17741 = CARTESIAN_POINT('Ctrl Pts',(86.4530062364447,51.6530790508433,24.6215623892904)) ;
#17742 = CARTESIAN_POINT('Ctrl Pts',(86.5165684565229,51.6005460069324,24.7)) ;
#17743 = CARTESIAN_POINT('',(86.3944620863754,51.7014647491801,25.8)) ;
#17744 = CARTESIAN_POINT('Origin',(86.6058929260522,51.6245102169318,25.8)) ;
#17745 = CARTESIAN_POINT('Origin',(84.75,52.3,24.55)) ;
#17746 = CARTESIAN_POINT('',(83.15,52.3,24.4)) ;
#17747 = CARTESIAN_POINT('Origin',(84.75,52.3,24.4)) ;
#17748 = CARTESIAN_POINT('',(83.,52.3,24.55)) ;
#17749 = CARTESIAN_POINT('',(83.,52.3,24.55)) ;
#17750 = CARTESIAN_POINT('Ctrl Pts',(83.,52.3,24.55)) ;
#17751 = CARTESIAN_POINT('Ctrl Pts',(82.9284376107081,52.3254444050815,24.6215623892919)) ;
#17752 = CARTESIAN_POINT('Ctrl Pts',(82.8507413023335,52.3530697591703,24.7)) ;
#17753 = CARTESIAN_POINT('',(83.0265864322286,52.6038843109171,24.55)) ;
#17754 = CARTESIAN_POINT('Ctrl Pts',(82.8703798425931,52.5775393014865,24.7)) ;
#17755 = CARTESIAN_POINT('Ctrl Pts',(82.9516928618558,52.5912531420121,24.6215623892918)) ;
#17756 = CARTESIAN_POINT('Ctrl Pts',(83.0265864322286,52.6038843109171,24.55)) ;
#17757 = CARTESIAN_POINT('Ctrl Pts',(83.0265864322286,52.6038843109171,24.55)) ;
#17758 = CARTESIAN_POINT('Ctrl Pts',(82.9605296110049,52.6413688368018,24.6215623892911)) ;
#17759 = CARTESIAN_POINT('Ctrl Pts',(82.8888107765314,52.6820663220492,24.7)) ;
#17760 = CARTESIAN_POINT('',(83.1055379136246,52.8985352508199,24.55)) ;
#17761 = CARTESIAN_POINT('Ctrl Pts',(82.9471296902017,52.8997154709092,24.7)) ;
#17762 = CARTESIAN_POINT('Ctrl Pts',(83.0295887654089,52.8991011097668,24.6215623892915)) ;
#17763 = CARTESIAN_POINT('Ctrl Pts',(83.1055379136246,52.8985352508199,24.55)) ;
#17764 = CARTESIAN_POINT('Ctrl Pts',(83.1055379136246,52.8985352508199,24.55)) ;
#17765 = CARTESIAN_POINT('Ctrl Pts',(83.0469937635528,52.9469209491587,24.6215623892935)) ;
#17766 = CARTESIAN_POINT('Ctrl Pts',(82.9834315434771,52.9994539930676,24.7)) ;
#17767 = CARTESIAN_POINT('',(83.2344555433772,53.175,24.55)) ;
#17768 = CARTESIAN_POINT('Ctrl Pts',(83.0786588398772,53.203669589219,24.7)) ;
#17769 = CARTESIAN_POINT('Ctrl Pts',(83.159758493753,53.1887456934613,24.621562389293)) ;
#17770 = CARTESIAN_POINT('Ctrl Pts',(83.2344555433772,53.175,24.55)) ;
#17771 = CARTESIAN_POINT('Ctrl Pts',(83.2344555433772,53.175,24.55)) ;
#17772 = CARTESIAN_POINT('Ctrl Pts',(83.185202898835,53.2328166958316,24.621562389293)) ;
#17773 = CARTESIAN_POINT('Ctrl Pts',(83.1317285990475,53.2955891084474,24.7)) ;
#17774 = CARTESIAN_POINT('',(83.4094222245417,53.4248783169514,24.55)) ;
#17775 = CARTESIAN_POINT('Ctrl Pts',(83.2609708449635,53.4801661643393,24.7)) ;
#17776 = CARTESIAN_POINT('Ctrl Pts',(83.3382469055668,53.4513861889864,24.6215623892912)) ;
#17777 = CARTESIAN_POINT('Ctrl Pts',(83.4094222245417,53.4248783169514,24.5500000000001)) ;
#17778 = CARTESIAN_POINT('Ctrl Pts',(83.4094222245417,53.4248783169514,24.55)) ;
#17779 = CARTESIAN_POINT('Ctrl Pts',(83.3709576022104,53.4903692792295,24.6215623892924)) ;
#17780 = CARTESIAN_POINT('Ctrl Pts',(83.3291960122509,53.5614737525594,24.7)) ;
#17781 = CARTESIAN_POINT('',(83.6251216830486,53.6405777754582,24.55)) ;
#17782 = CARTESIAN_POINT('Ctrl Pts',(83.4885262474406,53.7208039877491,24.7)) ;
#17783 = CARTESIAN_POINT('Ctrl Pts',(83.5596307207712,53.6790423977892,24.6215623892917)) ;
#17784 = CARTESIAN_POINT('Ctrl Pts',(83.6251216830486,53.6405777754582,24.55)) ;
#17785 = CARTESIAN_POINT('Ctrl Pts',(83.6251216830486,53.6405777754582,24.55)) ;
#17786 = CARTESIAN_POINT('Ctrl Pts',(83.5986138110136,53.7117530944334,24.6215623892914)) ;
#17787 = CARTESIAN_POINT('Ctrl Pts',(83.5698338356607,53.7890291550365,24.7)) ;
#17788 = CARTESIAN_POINT('',(83.875,53.8155444566228,24.55)) ;
#17789 = CARTESIAN_POINT('Ctrl Pts',(83.7544108915526,53.9182714009525,24.7)) ;
#17790 = CARTESIAN_POINT('Ctrl Pts',(83.8171833041694,53.8647971011641,24.6215623892916)) ;
#17791 = CARTESIAN_POINT('Ctrl Pts',(83.875,53.8155444566228,24.55)) ;
#17792 = CARTESIAN_POINT('Ctrl Pts',(83.875,53.8155444566228,24.55)) ;
#17793 = CARTESIAN_POINT('Ctrl Pts',(83.8612543065387,53.8902415062464,24.6215623892925)) ;
#17794 = CARTESIAN_POINT('Ctrl Pts',(83.846330410781,53.9713411601228,24.7)) ;
#17795 = CARTESIAN_POINT('',(84.1514647491801,53.9444620863754,24.55)) ;
#17796 = CARTESIAN_POINT('Ctrl Pts',(84.0505460069324,54.0665684565229,24.7)) ;
#17797 = CARTESIAN_POINT('Ctrl Pts',(84.1030790508414,54.003006236447,24.6215623892933)) ;
#17798 = CARTESIAN_POINT('Ctrl Pts',(84.1514647491801,53.9444620863754,24.55)) ;
#17799 = CARTESIAN_POINT('Ctrl Pts',(84.1514647491801,53.9444620863754,24.55)) ;
#17800 = CARTESIAN_POINT('Ctrl Pts',(84.1508988902332,54.0204112345913,24.6215623892916)) ;
#17801 = CARTESIAN_POINT('Ctrl Pts',(84.1502845290908,54.1028703097983,24.7)) ;
#17802 = CARTESIAN_POINT('',(84.4461156890829,54.0234135677714,24.55)) ;
#17803 = CARTESIAN_POINT('Ctrl Pts',(84.3679336779508,54.1611892234686,24.7)) ;
#17804 = CARTESIAN_POINT('Ctrl Pts',(84.4086311631982,54.089470388995,24.6215623892909)) ;
#17805 = CARTESIAN_POINT('Ctrl Pts',(84.4461156890829,54.0234135677714,24.55)) ;
#17806 = CARTESIAN_POINT('Ctrl Pts',(84.4461156890829,54.0234135677714,24.55)) ;
#17807 = CARTESIAN_POINT('Ctrl Pts',(84.4587468579881,54.0983071381452,24.6215623892927)) ;
#17808 = CARTESIAN_POINT('Ctrl Pts',(84.4724606985135,54.1796201574069,24.7)) ;
#17809 = CARTESIAN_POINT('',(84.75,54.05,24.55)) ;
#17810 = CARTESIAN_POINT('Ctrl Pts',(84.6969302408297,54.1992586976664,24.7)) ;
#17811 = CARTESIAN_POINT('Ctrl Pts',(84.724555594918,54.1215623892931,24.6215623892931)) ;
#17812 = CARTESIAN_POINT('Ctrl Pts',(84.75,54.05,24.55)) ;
#17813 = CARTESIAN_POINT('Ctrl Pts',(84.75,54.05,24.55)) ;
#17814 = CARTESIAN_POINT('Ctrl Pts',(84.7754444050815,54.1215623892917,24.6215623892917)) ;
#17815 = CARTESIAN_POINT('Ctrl Pts',(84.8030697591703,54.1992586976664,24.7)) ;
#17816 = CARTESIAN_POINT('',(85.0538843109171,54.0234135677714,24.55)) ;
#17817 = CARTESIAN_POINT('Ctrl Pts',(85.0275393014864,54.1796201574069,24.7)) ;
#17818 = CARTESIAN_POINT('Ctrl Pts',(85.041253142012,54.0983071381446,24.6215623892922)) ;
#17819 = CARTESIAN_POINT('Ctrl Pts',(85.0538843109171,54.0234135677714,24.55)) ;
#17820 = CARTESIAN_POINT('Ctrl Pts',(85.0538843109171,54.0234135677714,24.55)) ;
#17821 = CARTESIAN_POINT('Ctrl Pts',(85.0913688368026,54.0894703889965,24.6215623892926)) ;
#17822 = CARTESIAN_POINT('Ctrl Pts',(85.1320663220492,54.1611892234686,24.7)) ;
#17823 = CARTESIAN_POINT('',(85.3485352508199,53.9444620863754,24.55)) ;
#17824 = CARTESIAN_POINT('Ctrl Pts',(85.3497154709092,54.1028703097983,24.7)) ;
#17825 = CARTESIAN_POINT('Ctrl Pts',(85.3491011097668,54.0204112345911,24.6215623892915)) ;
#17826 = CARTESIAN_POINT('Ctrl Pts',(85.3485352508199,53.9444620863754,24.55)) ;
#17827 = CARTESIAN_POINT('Ctrl Pts',(85.3485352508199,53.9444620863754,24.55)) ;
#17828 = CARTESIAN_POINT('Ctrl Pts',(85.3969209491569,54.0030062364449,24.6215623892907)) ;
#17829 = CARTESIAN_POINT('Ctrl Pts',(85.4494539930676,54.0665684565229,24.7)) ;
#17830 = CARTESIAN_POINT('',(85.625,53.8155444566228,24.55)) ;
#17831 = CARTESIAN_POINT('Ctrl Pts',(85.653669589219,53.9713411601228,24.7)) ;
#17832 = CARTESIAN_POINT('Ctrl Pts',(85.6387456934611,53.890241506246,24.6215623892921)) ;
#17833 = CARTESIAN_POINT('Ctrl Pts',(85.625,53.8155444566228,24.55)) ;
#17834 = CARTESIAN_POINT('Ctrl Pts',(85.625,53.8155444566228,24.55)) ;
#17835 = CARTESIAN_POINT('Ctrl Pts',(85.6828166958308,53.8647971011643,24.6215623892919)) ;
#17836 = CARTESIAN_POINT('Ctrl Pts',(85.7455891084474,53.9182714009525,24.7)) ;
#17837 = CARTESIAN_POINT('',(85.8748783169514,53.6405777754582,24.55)) ;
#17838 = CARTESIAN_POINT('Ctrl Pts',(85.9301661643393,53.7890291550365,24.7)) ;
#17839 = CARTESIAN_POINT('Ctrl Pts',(85.9013861889865,53.7117530944334,24.6215623892915)) ;
#17840 = CARTESIAN_POINT('Ctrl Pts',(85.8748783169514,53.6405777754582,24.55)) ;
#17841 = CARTESIAN_POINT('Ctrl Pts',(85.8748783169514,53.6405777754582,24.55)) ;
#17842 = CARTESIAN_POINT('Ctrl Pts',(85.9403692792289,53.6790423977892,24.6215623892918)) ;
#17843 = CARTESIAN_POINT('Ctrl Pts',(86.0114737525594,53.7208039877491,24.7)) ;
#17844 = CARTESIAN_POINT('',(86.0905777754582,53.4248783169514,24.55)) ;
#17845 = CARTESIAN_POINT('Ctrl Pts',(86.1708039877491,53.5614737525594,24.7)) ;
#17846 = CARTESIAN_POINT('Ctrl Pts',(86.1290423977896,53.4903692792295,24.6215623892925)) ;
#17847 = CARTESIAN_POINT('Ctrl Pts',(86.0905777754582,53.4248783169514,24.55)) ;
#17848 = CARTESIAN_POINT('Ctrl Pts',(86.0905777754582,53.4248783169514,24.55)) ;
#17849 = CARTESIAN_POINT('Ctrl Pts',(86.1617530944339,53.4513861889867,24.621562389292)) ;
#17850 = CARTESIAN_POINT('Ctrl Pts',(86.2390291550365,53.4801661643393,24.7)) ;
#17851 = CARTESIAN_POINT('',(86.2655444566228,53.175,24.55)) ;
#17852 = CARTESIAN_POINT('Ctrl Pts',(86.3682714009525,53.2955891084474,24.7)) ;
#17853 = CARTESIAN_POINT('Ctrl Pts',(86.3147971011637,53.2328166958301,24.6215623892911)) ;
#17854 = CARTESIAN_POINT('Ctrl Pts',(86.2655444566228,53.175,24.55)) ;
#17855 = CARTESIAN_POINT('Ctrl Pts',(86.2655444566228,53.175,24.55)) ;
#17856 = CARTESIAN_POINT('Ctrl Pts',(86.3402415062452,53.188745693461,24.6215623892913)) ;
#17857 = CARTESIAN_POINT('Ctrl Pts',(86.4213411601228,53.203669589219,24.7)) ;
#17858 = CARTESIAN_POINT('',(86.3944620863754,52.8985352508199,24.55)) ;
#17859 = CARTESIAN_POINT('Ctrl Pts',(86.5165684565229,52.9994539930676,24.7)) ;
#17860 = CARTESIAN_POINT('Ctrl Pts',(86.4530062364461,52.9469209491579,24.6215623892922)) ;
#17861 = CARTESIAN_POINT('Ctrl Pts',(86.3944620863754,52.8985352508199,24.55)) ;
#17862 = CARTESIAN_POINT('Ctrl Pts',(86.3944620863754,52.8985352508199,24.55)) ;
#17863 = CARTESIAN_POINT('Ctrl Pts',(86.4704112345918,52.8991011097668,24.6215623892921)) ;
#17864 = CARTESIAN_POINT('Ctrl Pts',(86.5528703097983,52.8997154709092,24.7)) ;
#17865 = CARTESIAN_POINT('',(86.4734135677714,52.6038843109171,24.55)) ;
#17866 = CARTESIAN_POINT('Ctrl Pts',(86.6111892234686,52.6820663220492,24.7)) ;
#17867 = CARTESIAN_POINT('Ctrl Pts',(86.539470388997,52.6413688368029,24.6215623892932)) ;
#17868 = CARTESIAN_POINT('Ctrl Pts',(86.4734135677714,52.6038843109171,24.55)) ;
#17869 = CARTESIAN_POINT('Ctrl Pts',(86.4734135677714,52.6038843109171,24.55)) ;
#17870 = CARTESIAN_POINT('Ctrl Pts',(86.5483071381438,52.5912531420121,24.6215623892914)) ;
#17871 = CARTESIAN_POINT('Ctrl Pts',(86.6296201574069,52.5775393014865,24.7)) ;
#17872 = CARTESIAN_POINT('',(86.5,52.3,24.55)) ;
#17873 = CARTESIAN_POINT('Ctrl Pts',(86.6492586976664,52.3530697591703,24.7)) ;
#17874 = CARTESIAN_POINT('Ctrl Pts',(86.571562389291,52.3254444050812,24.621562389291)) ;
#17875 = CARTESIAN_POINT('Ctrl Pts',(86.5,52.3,24.55)) ;
#17876 = CARTESIAN_POINT('Ctrl Pts',(86.5,52.3,24.55)) ;
#17877 = CARTESIAN_POINT('Ctrl Pts',(86.5715623892916,52.2745555949185,24.6215623892916)) ;
#17878 = CARTESIAN_POINT('Ctrl Pts',(86.6492586976664,52.2469302408297,24.7)) ;
#17879 = CARTESIAN_POINT('',(86.2655444566228,51.425,24.55)) ;
#17880 = CARTESIAN_POINT('Ctrl Pts',(86.4213411601228,51.396330410781,24.7)) ;
#17881 = CARTESIAN_POINT('Ctrl Pts',(86.340241506248,51.4112543065385,24.621562389294)) ;
#17882 = CARTESIAN_POINT('Ctrl Pts',(86.2655444566228,51.425,24.55)) ;
#17883 = CARTESIAN_POINT('Ctrl Pts',(86.2655444566228,51.425,24.55)) ;
#17884 = CARTESIAN_POINT('Ctrl Pts',(86.3147971011642,51.3671833041693,24.6215623892918)) ;
#17885 = CARTESIAN_POINT('Ctrl Pts',(86.3682714009526,51.3044108915526,24.7)) ;
#17886 = CARTESIAN_POINT('',(86.0905777754582,51.1751216830486,24.55)) ;
#17887 = CARTESIAN_POINT('Ctrl Pts',(86.2390291550365,51.1198338356607,24.7)) ;
#17888 = CARTESIAN_POINT('Ctrl Pts',(86.1617530944332,51.1486138110136,24.6215623892913)) ;
#17889 = CARTESIAN_POINT('Ctrl Pts',(86.0905777754582,51.1751216830486,24.55)) ;
#17890 = CARTESIAN_POINT('Ctrl Pts',(86.0905777754582,51.1751216830486,24.55)) ;
#17891 = CARTESIAN_POINT('Ctrl Pts',(86.1290423977896,51.1096307207706,24.6215623892924)) ;
#17892 = CARTESIAN_POINT('Ctrl Pts',(86.1708039877491,51.0385262474406,24.7)) ;
#17893 = CARTESIAN_POINT('',(85.8748783169514,50.9594222245418,24.55)) ;
#17894 = CARTESIAN_POINT('Ctrl Pts',(86.0114737525595,50.8791960122509,24.7)) ;
#17895 = CARTESIAN_POINT('Ctrl Pts',(85.940369279228,50.9209576022113,24.6215623892908)) ;
#17896 = CARTESIAN_POINT('Ctrl Pts',(85.8748783169514,50.9594222245418,24.55)) ;
#17897 = CARTESIAN_POINT('Ctrl Pts',(85.8748783169514,50.9594222245418,24.55)) ;
#17898 = CARTESIAN_POINT('Ctrl Pts',(85.9013861889867,50.8882469055658,24.6215623892922)) ;
#17899 = CARTESIAN_POINT('Ctrl Pts',(85.9301661643393,50.8109708449635,24.7)) ;
#17900 = CARTESIAN_POINT('',(85.625,50.7844555433772,24.55)) ;
#17901 = CARTESIAN_POINT('Ctrl Pts',(85.7455891084474,50.6817285990474,24.7)) ;
#17902 = CARTESIAN_POINT('Ctrl Pts',(85.6828166958308,50.7352028988357,24.6215623892919)) ;
#17903 = CARTESIAN_POINT('Ctrl Pts',(85.625,50.7844555433772,24.55)) ;
#17904 = CARTESIAN_POINT('Ctrl Pts',(85.625,50.7844555433772,24.55)) ;
#17905 = CARTESIAN_POINT('Ctrl Pts',(85.6387456934614,50.7097584937526,24.6215623892934)) ;
#17906 = CARTESIAN_POINT('Ctrl Pts',(85.653669589219,50.6286588398772,24.7)) ;
#17907 = CARTESIAN_POINT('',(85.3485352508199,50.6555379136246,24.55)) ;
#17908 = CARTESIAN_POINT('Ctrl Pts',(85.4494539930676,50.5334315434771,24.7)) ;
#17909 = CARTESIAN_POINT('Ctrl Pts',(85.3969209491577,50.5969937635541,24.6215623892919)) ;
#17910 = CARTESIAN_POINT('Ctrl Pts',(85.3485352508199,50.6555379136246,24.55)) ;
#17911 = CARTESIAN_POINT('Ctrl Pts',(85.3485352508199,50.6555379136246,24.55)) ;
#17912 = CARTESIAN_POINT('Ctrl Pts',(85.3491011097668,50.5795887654084,24.6215623892919)) ;
#17913 = CARTESIAN_POINT('Ctrl Pts',(85.3497154709092,50.4971296902017,24.7)) ;
#17914 = CARTESIAN_POINT('',(85.0538843109171,50.5765864322286,24.55)) ;
#17915 = CARTESIAN_POINT('Ctrl Pts',(85.1320663220493,50.4388107765314,24.7)) ;
#17916 = CARTESIAN_POINT('Ctrl Pts',(85.0913688368028,50.5105296110033,24.6215623892928)) ;
#17917 = CARTESIAN_POINT('Ctrl Pts',(85.0538843109171,50.5765864322286,24.55)) ;
#17918 = CARTESIAN_POINT('Ctrl Pts',(85.0538843109171,50.5765864322286,24.55)) ;
#17919 = CARTESIAN_POINT('Ctrl Pts',(85.041253142012,50.5016928618549,24.6215623892927)) ;
#17920 = CARTESIAN_POINT('Ctrl Pts',(85.0275393014865,50.4203798425931,24.7)) ;
#17921 = CARTESIAN_POINT('',(84.75,50.55,24.55)) ;
#17922 = CARTESIAN_POINT('Ctrl Pts',(84.8030697591703,50.4007413023336,24.7)) ;
#17923 = CARTESIAN_POINT('Ctrl Pts',(84.7754444050818,50.4784376107076,24.6215623892924)) ;
#17924 = CARTESIAN_POINT('Ctrl Pts',(84.75,50.55,24.55)) ;
#17925 = CARTESIAN_POINT('Ctrl Pts',(84.75,50.55,24.55)) ;
#17926 = CARTESIAN_POINT('Ctrl Pts',(84.7245555949187,50.4784376107088,24.6215623892912)) ;
#17927 = CARTESIAN_POINT('Ctrl Pts',(84.6969302408297,50.4007413023336,24.7)) ;
#17928 = CARTESIAN_POINT('',(84.4461156890829,50.5765864322286,24.55)) ;
#17929 = CARTESIAN_POINT('Ctrl Pts',(84.4724606985135,50.4203798425931,24.7)) ;
#17930 = CARTESIAN_POINT('Ctrl Pts',(84.458746857988,50.5016928618554,24.6215623892922)) ;
#17931 = CARTESIAN_POINT('Ctrl Pts',(84.4461156890829,50.5765864322286,24.55)) ;
#17932 = CARTESIAN_POINT('Ctrl Pts',(84.4461156890829,50.5765864322286,24.55)) ;
#17933 = CARTESIAN_POINT('Ctrl Pts',(84.4086311631976,50.5105296110039,24.6215623892921)) ;
#17934 = CARTESIAN_POINT('Ctrl Pts',(84.3679336779508,50.4388107765314,24.7)) ;
#17935 = CARTESIAN_POINT('',(84.1514647491801,50.6555379136246,24.55)) ;
#17936 = CARTESIAN_POINT('Ctrl Pts',(84.1502845290908,50.4971296902017,24.7)) ;
#17937 = CARTESIAN_POINT('Ctrl Pts',(84.1508988902331,50.5795887654091,24.6215623892912)) ;
#17938 = CARTESIAN_POINT('Ctrl Pts',(84.1514647491801,50.6555379136246,24.55)) ;
#17939 = CARTESIAN_POINT('Ctrl Pts',(84.1514647491801,50.6555379136246,24.55)) ;
#17940 = CARTESIAN_POINT('Ctrl Pts',(84.1030790508424,50.5969937635541,24.6215623892919)) ;
#17941 = CARTESIAN_POINT('Ctrl Pts',(84.0505460069324,50.5334315434771,24.7)) ;
#17942 = CARTESIAN_POINT('',(83.875,50.7844555433772,24.55)) ;
#17943 = CARTESIAN_POINT('Ctrl Pts',(83.846330410781,50.6286588398772,24.7)) ;
#17944 = CARTESIAN_POINT('Ctrl Pts',(83.8612543065388,50.7097584937536,24.6215623892925)) ;
#17945 = CARTESIAN_POINT('Ctrl Pts',(83.875,50.7844555433772,24.55)) ;
#17946 = CARTESIAN_POINT('Ctrl Pts',(83.875,50.7844555433772,24.55)) ;
#17947 = CARTESIAN_POINT('Ctrl Pts',(83.8171833041691,50.7352028988356,24.621562389292)) ;
#17948 = CARTESIAN_POINT('Ctrl Pts',(83.7544108915526,50.6817285990475,24.7)) ;
#17949 = CARTESIAN_POINT('',(83.6251216830486,50.9594222245418,24.55)) ;
#17950 = CARTESIAN_POINT('Ctrl Pts',(83.5698338356607,50.8109708449635,24.7)) ;
#17951 = CARTESIAN_POINT('Ctrl Pts',(83.5986138110132,50.8882469055657,24.6215623892923)) ;
#17952 = CARTESIAN_POINT('Ctrl Pts',(83.6251216830486,50.9594222245418,24.55)) ;
#17953 = CARTESIAN_POINT('Ctrl Pts',(83.6251216830486,50.9594222245418,24.55)) ;
#17954 = CARTESIAN_POINT('Ctrl Pts',(83.5596307207711,50.9209576022107,24.6215623892917)) ;
#17955 = CARTESIAN_POINT('Ctrl Pts',(83.4885262474406,50.8791960122509,24.7)) ;
#17956 = CARTESIAN_POINT('',(83.4094222245418,51.1751216830486,24.55)) ;
#17957 = CARTESIAN_POINT('Ctrl Pts',(83.3291960122509,51.0385262474406,24.7)) ;
#17958 = CARTESIAN_POINT('Ctrl Pts',(83.3709576022109,51.1096307207714,24.6215623892914)) ;
#17959 = CARTESIAN_POINT('Ctrl Pts',(83.4094222245418,51.1751216830486,24.55)) ;
#17960 = CARTESIAN_POINT('Ctrl Pts',(83.4094222245418,51.1751216830486,24.55)) ;
#17961 = CARTESIAN_POINT('Ctrl Pts',(83.3382469055639,51.1486138110125,24.6215623892941)) ;
#17962 = CARTESIAN_POINT('Ctrl Pts',(83.2609708449635,51.1198338356607,24.7)) ;
#17963 = CARTESIAN_POINT('',(83.2344555433772,51.425,24.55)) ;
#17964 = CARTESIAN_POINT('Ctrl Pts',(83.1317285990474,51.3044108915526,24.7)) ;
#17965 = CARTESIAN_POINT('Ctrl Pts',(83.1852028988347,51.3671833041681,24.6215623892934)) ;
#17966 = CARTESIAN_POINT('Ctrl Pts',(83.2344555433772,51.425,24.55)) ;
#17967 = CARTESIAN_POINT('Ctrl Pts',(83.2344555433772,51.425,24.55)) ;
#17968 = CARTESIAN_POINT('Ctrl Pts',(83.1597584937539,51.4112543065388,24.6215623892922)) ;
#17969 = CARTESIAN_POINT('Ctrl Pts',(83.0786588398772,51.396330410781,24.7)) ;
#17970 = CARTESIAN_POINT('',(83.1055379136246,51.7014647491801,24.55)) ;
#17971 = CARTESIAN_POINT('Ctrl Pts',(82.9834315434771,51.6005460069324,24.7)) ;
#17972 = CARTESIAN_POINT('Ctrl Pts',(83.0469937635532,51.6530790508416,24.621562389293)) ;
#17973 = CARTESIAN_POINT('Ctrl Pts',(83.1055379136246,51.7014647491801,24.55)) ;
#17974 = CARTESIAN_POINT('Ctrl Pts',(83.1055379136246,51.7014647491801,24.55)) ;
#17975 = CARTESIAN_POINT('Ctrl Pts',(83.0295887654081,51.7008988902332,24.6215623892922)) ;
#17976 = CARTESIAN_POINT('Ctrl Pts',(82.9471296902017,51.7002845290908,24.7)) ;
#17977 = CARTESIAN_POINT('',(83.0265864322286,51.9961156890829,24.55)) ;
#17978 = CARTESIAN_POINT('Ctrl Pts',(82.8888107765314,51.9179336779508,24.7)) ;
#17979 = CARTESIAN_POINT('Ctrl Pts',(82.9605296110043,51.9586311631978,24.6215623892918)) ;
#17980 = CARTESIAN_POINT('Ctrl Pts',(83.0265864322286,51.9961156890829,24.55)) ;
#17981 = CARTESIAN_POINT('Ctrl Pts',(83.0265864322286,51.9961156890829,24.55)) ;
#17982 = CARTESIAN_POINT('Ctrl Pts',(82.9516928618564,52.0087468579878,24.6215623892912)) ;
#17983 = CARTESIAN_POINT('Ctrl Pts',(82.8703798425931,52.0224606985135,24.7)) ;
#17984 = CARTESIAN_POINT('Ctrl Pts',(82.8507413023335,52.2469302408297,24.7)) ;
#17985 = CARTESIAN_POINT('Ctrl Pts',(82.928437610706,52.2745555949177,24.621562389294)) ;
#17986 = CARTESIAN_POINT('Ctrl Pts',(83.,52.3,24.55)) ;
#17987 = CARTESIAN_POINT('Origin',(86.4604001724743,51.3125,25.8)) ;
#17988 = CARTESIAN_POINT('',(86.2655444566228,51.425,25.8)) ;
#17989 = CARTESIAN_POINT('',(86.2655444566228,51.425,25.8)) ;
#17990 = CARTESIAN_POINT('',(86.7352558883258,51.3385640646055,25.8)) ;
#17991 = CARTESIAN_POINT('Origin',(86.7352558883258,51.3385640646055,24.4)) ;
#17992 = CARTESIAN_POINT('',(86.2655444566228,51.425,24.4)) ;
#17993 = CARTESIAN_POINT('Origin',(86.2655444566228,51.425,24.4)) ;
#17994 = CARTESIAN_POINT('Origin',(86.5381437924116,51.0084343695886,24.4)) ;
#17995 = CARTESIAN_POINT('',(86.0905777754582,51.1751216830486,25.8)) ;
#17996 = CARTESIAN_POINT('',(86.5381437924116,51.0084343695886,25.8)) ;
#17997 = CARTESIAN_POINT('',(86.0905777754582,51.1751216830486,24.4)) ;
#17998 = CARTESIAN_POINT('Origin',(86.0905777754582,51.1751216830486,24.4)) ;
#17999 = CARTESIAN_POINT('',(86.0905777754582,51.1751216830486,25.8)) ;
#18000 = CARTESIAN_POINT('Origin',(86.26293777516,51.0304944708691,25.8)) ;
#18001 = CARTESIAN_POINT('Origin',(86.0195055291309,50.78706222484,25.8)) ;
#18002 = CARTESIAN_POINT('',(85.8748783169514,50.9594222245418,25.8)) ;
#18003 = CARTESIAN_POINT('',(85.8748783169514,50.9594222245418,25.8)) ;
#18004 = CARTESIAN_POINT('',(86.2866998522094,50.7175482426881,25.8)) ;
#18005 = CARTESIAN_POINT('Origin',(86.2866998522094,50.7175482426881,24.4)) ;
#18006 = CARTESIAN_POINT('',(85.8748783169514,50.9594222245418,24.4)) ;
#18007 = CARTESIAN_POINT('Origin',(85.8748783169514,50.9594222245418,24.4)) ;
#18008 = CARTESIAN_POINT('Origin',(85.9885640646055,50.4747441116742,24.4)) ;
#18009 = CARTESIAN_POINT('',(85.625,50.7844555433772,25.8)) ;
#18010 = CARTESIAN_POINT('',(85.9885640646055,50.4747441116742,25.8)) ;
#18011 = CARTESIAN_POINT('',(85.625,50.7844555433772,24.4)) ;
#18012 = CARTESIAN_POINT('Origin',(85.625,50.7844555433772,24.4)) ;
#18013 = CARTESIAN_POINT('',(85.625,50.7844555433772,25.8)) ;
#18014 = CARTESIAN_POINT('Origin',(85.7375,50.5895998275257,25.8)) ;
#18015 = CARTESIAN_POINT('Origin',(85.4254897830682,50.4441070739478,25.8)) ;
#18016 = CARTESIAN_POINT('',(85.3485352508199,50.6555379136246,25.8)) ;
#18017 = CARTESIAN_POINT('',(85.3485352508199,50.6555379136246,25.8)) ;
#18018 = CARTESIAN_POINT('',(85.6527951346422,50.2873994572031,25.8)) ;
#18019 = CARTESIAN_POINT('Origin',(85.6527951346422,50.2873994572031,24.4)) ;
#18020 = CARTESIAN_POINT('',(85.3485352508199,50.6555379136246,24.4)) ;
#18021 = CARTESIAN_POINT('Origin',(85.3485352508199,50.6555379136246,24.4)) ;
#18022 = CARTESIAN_POINT('Origin',(85.2895952313492,50.1612066517998,24.4)) ;
#18023 = CARTESIAN_POINT('',(85.0538843109171,50.5765864322286,25.8)) ;
#18024 = CARTESIAN_POINT('',(85.2895952313492,50.1612066517998,25.8)) ;
#18025 = CARTESIAN_POINT('',(85.0538843109171,50.5765864322286,24.4)) ;
#18026 = CARTESIAN_POINT('Origin',(85.0538843109171,50.5765864322286,24.4)) ;
#18027 = CARTESIAN_POINT('',(85.0538843109171,50.5765864322286,25.8)) ;
#18028 = CARTESIAN_POINT('Origin',(85.0929551508922,50.3550046878009,25.8)) ;
#18029 = CARTESIAN_POINT('Origin',(84.75,50.325,25.8)) ;
#18030 = CARTESIAN_POINT('',(84.75,50.55,25.8)) ;
#18031 = CARTESIAN_POINT('',(84.75,50.55,25.8)) ;
#18032 = CARTESIAN_POINT('',(84.91,50.1,25.8)) ;
#18033 = CARTESIAN_POINT('Origin',(84.91,50.1,24.4)) ;
#18034 = CARTESIAN_POINT('',(84.75,50.55,24.4)) ;
#18035 = CARTESIAN_POINT('Origin',(84.75,50.55,24.4)) ;
#18036 = CARTESIAN_POINT('Origin',(84.5255432496147,50.1056392349464,24.4)) ;
#18037 = CARTESIAN_POINT('',(84.4461156890829,50.5765864322286,25.8)) ;
#18038 = CARTESIAN_POINT('',(84.5255432496147,50.1056392349464,25.8)) ;
#18039 = CARTESIAN_POINT('',(84.4461156890829,50.5765864322286,24.4)) ;
#18040 = CARTESIAN_POINT('Origin',(84.4461156890829,50.5765864322286,24.4)) ;
#18041 = CARTESIAN_POINT('',(84.4461156890829,50.5765864322286,25.8)) ;
#18042 = CARTESIAN_POINT('Origin',(84.4070448491078,50.3550046878009,25.8)) ;
#18043 = CARTESIAN_POINT('Origin',(84.0745102169318,50.4441070739478,25.8)) ;
#18044 = CARTESIAN_POINT('',(84.1514647491801,50.6555379136246,25.8)) ;
#18045 = CARTESIAN_POINT('',(84.1514647491801,50.6555379136246,25.8)) ;
#18046 = CARTESIAN_POINT('',(84.1479065040093,50.1779530113389,25.8)) ;
#18047 = CARTESIAN_POINT('Origin',(84.1479065040093,50.1779530113389,24.4)) ;
#18048 = CARTESIAN_POINT('',(84.1514647491801,50.6555379136246,24.4)) ;
#18049 = CARTESIAN_POINT('Origin',(84.1514647491801,50.6555379136246,24.4)) ;
#18050 = CARTESIAN_POINT('Origin',(83.7885640646055,50.3147441116742,24.4)) ;
#18051 = CARTESIAN_POINT('',(83.875,50.7844555433772,25.8)) ;
#18052 = CARTESIAN_POINT('',(83.7885640646055,50.3147441116742,25.8)) ;
#18053 = CARTESIAN_POINT('',(83.875,50.7844555433772,24.4)) ;
#18054 = CARTESIAN_POINT('Origin',(83.875,50.7844555433772,24.4)) ;
#18055 = CARTESIAN_POINT('',(83.875,50.7844555433772,25.8)) ;
#18056 = CARTESIAN_POINT('Origin',(83.7625,50.5895998275257,25.8)) ;
#18057 = CARTESIAN_POINT('Origin',(83.4804944708691,50.78706222484,25.8)) ;
#18058 = CARTESIAN_POINT('',(83.6251216830486,50.9594222245418,25.8)) ;
#18059 = CARTESIAN_POINT('',(83.6251216830486,50.9594222245418,25.8)) ;
#18060 = CARTESIAN_POINT('',(83.4584343695887,50.5118562075884,25.8)) ;
#18061 = CARTESIAN_POINT('Origin',(83.4584343695887,50.5118562075884,24.4)) ;
#18062 = CARTESIAN_POINT('',(83.6251216830486,50.9594222245418,24.4)) ;
#18063 = CARTESIAN_POINT('Origin',(83.6251216830486,50.9594222245418,24.4)) ;
#18064 = CARTESIAN_POINT('Origin',(83.1675482426881,50.7633001477906,24.4)) ;
#18065 = CARTESIAN_POINT('',(83.4094222245418,51.1751216830486,25.8)) ;
#18066 = CARTESIAN_POINT('',(83.1675482426881,50.7633001477906,25.8)) ;
#18067 = CARTESIAN_POINT('',(83.4094222245418,51.1751216830486,24.4)) ;
#18068 = CARTESIAN_POINT('Origin',(83.4094222245418,51.1751216830486,24.4)) ;
#18069 = CARTESIAN_POINT('',(83.4094222245418,51.1751216830486,25.8)) ;
#18070 = CARTESIAN_POINT('Origin',(83.23706222484,51.0304944708691,25.8)) ;
#18071 = CARTESIAN_POINT('Origin',(83.0395998275257,51.3125,25.8)) ;
#18072 = CARTESIAN_POINT('',(83.2344555433772,51.425,25.8)) ;
#18073 = CARTESIAN_POINT('',(83.2344555433772,51.425,25.8)) ;
#18074 = CARTESIAN_POINT('',(82.9247441116742,51.0614359353945,25.8)) ;
#18075 = CARTESIAN_POINT('Origin',(82.9247441116742,51.0614359353945,24.4)) ;
#18076 = CARTESIAN_POINT('',(83.2344555433772,51.425,24.4)) ;
#18077 = CARTESIAN_POINT('Origin',(83.2344555433772,51.425,24.4)) ;
#18078 = CARTESIAN_POINT('Origin',(82.7373994572031,51.3972048653578,24.4)) ;
#18079 = CARTESIAN_POINT('',(83.1055379136246,51.7014647491801,25.8)) ;
#18080 = CARTESIAN_POINT('',(82.7373994572031,51.3972048653578,25.8)) ;
#18081 = CARTESIAN_POINT('',(83.1055379136246,51.7014647491801,24.4)) ;
#18082 = CARTESIAN_POINT('Origin',(83.1055379136246,51.7014647491801,24.4)) ;
#18083 = CARTESIAN_POINT('',(83.1055379136246,51.7014647491801,25.8)) ;
#18084 = CARTESIAN_POINT('Origin',(82.8941070739478,51.6245102169318,25.8)) ;
#18085 = CARTESIAN_POINT('Origin',(82.8050046878009,51.9570448491078,25.8)) ;
#18086 = CARTESIAN_POINT('',(83.0265864322286,51.9961156890829,25.8)) ;
#18087 = CARTESIAN_POINT('',(83.0265864322286,51.9961156890829,25.8)) ;
#18088 = CARTESIAN_POINT('',(82.6112066517998,51.7604047686508,25.8)) ;
#18089 = CARTESIAN_POINT('Origin',(82.6112066517998,51.7604047686508,24.4)) ;
#18090 = CARTESIAN_POINT('',(83.0265864322286,51.9961156890829,24.4)) ;
#18091 = CARTESIAN_POINT('Origin',(83.0265864322286,51.9961156890829,24.4)) ;
#18092 = CARTESIAN_POINT('Origin',(82.55,52.14,24.4)) ;
#18093 = CARTESIAN_POINT('',(83.,52.3,25.8)) ;
#18094 = CARTESIAN_POINT('',(82.55,52.14,25.8)) ;
#18095 = CARTESIAN_POINT('',(83.,52.3,24.4)) ;
#18096 = CARTESIAN_POINT('Origin',(83.,52.3,24.4)) ;
#18097 = CARTESIAN_POINT('',(83.,52.3,25.8)) ;
#18098 = CARTESIAN_POINT('Origin',(82.775,52.3,25.8)) ;
#18099 = CARTESIAN_POINT('Origin',(82.8050046878009,52.6429551508922,25.8)) ;
#18100 = CARTESIAN_POINT('',(83.0265864322286,52.6038843109171,25.8)) ;
#18101 = CARTESIAN_POINT('',(83.0265864322286,52.6038843109171,25.8)) ;
#18102 = CARTESIAN_POINT('',(82.5556392349464,52.5244567503853,25.8)) ;
#18103 = CARTESIAN_POINT('Origin',(82.5556392349464,52.5244567503853,24.4)) ;
#18104 = CARTESIAN_POINT('',(83.0265864322286,52.6038843109171,24.4)) ;
#18105 = CARTESIAN_POINT('Origin',(83.0265864322286,52.6038843109171,24.4)) ;
#18106 = CARTESIAN_POINT('Origin',(82.6279530113389,52.9020934959907,24.4)) ;
#18107 = CARTESIAN_POINT('',(83.1055379136246,52.8985352508199,25.8)) ;
#18108 = CARTESIAN_POINT('',(82.6279530113389,52.9020934959907,25.8)) ;
#18109 = CARTESIAN_POINT('',(83.1055379136246,52.8985352508199,24.4)) ;
#18110 = CARTESIAN_POINT('Origin',(83.1055379136246,52.8985352508199,24.4)) ;
#18111 = CARTESIAN_POINT('',(83.1055379136246,52.8985352508199,25.8)) ;
#18112 = CARTESIAN_POINT('Origin',(82.8941070739478,52.9754897830682,25.8)) ;
#18113 = CARTESIAN_POINT('Origin',(83.0395998275257,53.2875,25.8)) ;
#18114 = CARTESIAN_POINT('',(83.2344555433772,53.175,25.8)) ;
#18115 = CARTESIAN_POINT('',(83.2344555433772,53.175,25.8)) ;
#18116 = CARTESIAN_POINT('',(82.7647441116742,53.2614359353945,25.8)) ;
#18117 = CARTESIAN_POINT('Origin',(82.7647441116742,53.2614359353945,24.4)) ;
#18118 = CARTESIAN_POINT('',(83.2344555433772,53.175,24.4)) ;
#18119 = CARTESIAN_POINT('Origin',(83.2344555433772,53.175,24.4)) ;
#18120 = CARTESIAN_POINT('Origin',(82.9618562075884,53.5915656304114,24.4)) ;
#18121 = CARTESIAN_POINT('',(83.4094222245417,53.4248783169514,25.8)) ;
#18122 = CARTESIAN_POINT('',(82.9618562075884,53.5915656304114,25.8)) ;
#18123 = CARTESIAN_POINT('',(83.4094222245417,53.4248783169514,24.4)) ;
#18124 = CARTESIAN_POINT('Origin',(83.4094222245417,53.4248783169514,24.4)) ;
#18125 = CARTESIAN_POINT('',(83.4094222245417,53.4248783169514,25.8)) ;
#18126 = CARTESIAN_POINT('Origin',(83.23706222484,53.5695055291309,25.8)) ;
#18127 = CARTESIAN_POINT('Origin',(83.4804944708691,53.81293777516,25.8)) ;
#18128 = CARTESIAN_POINT('',(83.6251216830486,53.6405777754582,25.8)) ;
#18129 = CARTESIAN_POINT('',(83.6251216830486,53.6405777754582,25.8)) ;
#18130 = CARTESIAN_POINT('',(83.2133001477906,53.8824517573119,25.8)) ;
#18131 = CARTESIAN_POINT('Origin',(83.2133001477906,53.8824517573119,24.4)) ;
#18132 = CARTESIAN_POINT('',(83.6251216830486,53.6405777754582,24.4)) ;
#18133 = CARTESIAN_POINT('Origin',(83.6251216830486,53.6405777754582,24.4)) ;
#18134 = CARTESIAN_POINT('Origin',(83.5114359353945,54.1252558883258,24.4)) ;
#18135 = CARTESIAN_POINT('',(83.875,53.8155444566228,25.8)) ;
#18136 = CARTESIAN_POINT('',(83.5114359353945,54.1252558883258,25.8)) ;
#18137 = CARTESIAN_POINT('',(83.875,53.8155444566228,24.4)) ;
#18138 = CARTESIAN_POINT('Origin',(83.875,53.8155444566228,24.4)) ;
#18139 = CARTESIAN_POINT('',(83.875,53.8155444566228,25.8)) ;
#18140 = CARTESIAN_POINT('Origin',(83.7625,54.0104001724743,25.8)) ;
#18141 = CARTESIAN_POINT('Origin',(84.0745102169318,54.1558929260522,25.8)) ;
#18142 = CARTESIAN_POINT('',(84.1514647491801,53.9444620863754,25.8)) ;
#18143 = CARTESIAN_POINT('',(84.1514647491801,53.9444620863754,25.8)) ;
#18144 = CARTESIAN_POINT('',(83.8472048653578,54.3126005427969,25.8)) ;
#18145 = CARTESIAN_POINT('Origin',(83.8472048653578,54.3126005427969,24.4)) ;
#18146 = CARTESIAN_POINT('',(84.1514647491801,53.9444620863754,24.4)) ;
#18147 = CARTESIAN_POINT('Origin',(84.1514647491801,53.9444620863754,24.4)) ;
#18148 = CARTESIAN_POINT('Origin',(84.2104047686508,54.4387933482002,24.4)) ;
#18149 = CARTESIAN_POINT('',(84.4461156890829,54.0234135677714,25.8)) ;
#18150 = CARTESIAN_POINT('',(84.2104047686508,54.4387933482002,25.8)) ;
#18151 = CARTESIAN_POINT('',(84.4461156890829,54.0234135677714,24.4)) ;
#18152 = CARTESIAN_POINT('Origin',(84.4461156890829,54.0234135677714,24.4)) ;
#18153 = CARTESIAN_POINT('',(84.4461156890829,54.0234135677714,25.8)) ;
#18154 = CARTESIAN_POINT('Origin',(84.4070448491078,54.2449953121991,25.8)) ;
#18155 = CARTESIAN_POINT('Origin',(84.75,54.275,25.8)) ;
#18156 = CARTESIAN_POINT('',(84.75,54.05,25.8)) ;
#18157 = CARTESIAN_POINT('',(84.75,54.05,25.8)) ;
#18158 = CARTESIAN_POINT('',(84.59,54.5,25.8)) ;
#18159 = CARTESIAN_POINT('Origin',(84.59,54.5,24.4)) ;
#18160 = CARTESIAN_POINT('',(84.75,54.05,24.4)) ;
#18161 = CARTESIAN_POINT('Origin',(84.75,54.05,24.4)) ;
#18162 = CARTESIAN_POINT('Origin',(84.9744567503853,54.4943607650536,24.4)) ;
#18163 = CARTESIAN_POINT('',(85.0538843109171,54.0234135677714,25.8)) ;
#18164 = CARTESIAN_POINT('',(84.9744567503853,54.4943607650536,25.8)) ;
#18165 = CARTESIAN_POINT('',(85.0538843109171,54.0234135677714,24.4)) ;
#18166 = CARTESIAN_POINT('Origin',(85.0538843109171,54.0234135677714,24.4)) ;
#18167 = CARTESIAN_POINT('',(85.0538843109171,54.0234135677714,25.8)) ;
#18168 = CARTESIAN_POINT('Origin',(85.0929551508922,54.2449953121991,25.8)) ;
#18169 = CARTESIAN_POINT('Origin',(85.4254897830682,54.1558929260522,25.8)) ;
#18170 = CARTESIAN_POINT('',(85.3485352508199,53.9444620863754,25.8)) ;
#18171 = CARTESIAN_POINT('',(85.3485352508199,53.9444620863754,25.8)) ;
#18172 = CARTESIAN_POINT('',(85.3520934959907,54.4220469886611,25.8)) ;
#18173 = CARTESIAN_POINT('Origin',(85.3520934959907,54.4220469886611,24.4)) ;
#18174 = CARTESIAN_POINT('',(85.3485352508199,53.9444620863754,24.4)) ;
#18175 = CARTESIAN_POINT('Origin',(85.3485352508199,53.9444620863754,24.4)) ;
#18176 = CARTESIAN_POINT('Origin',(85.7114359353945,54.2852558883258,24.4)) ;
#18177 = CARTESIAN_POINT('',(85.625,53.8155444566228,25.8)) ;
#18178 = CARTESIAN_POINT('',(85.7114359353945,54.2852558883258,25.8)) ;
#18179 = CARTESIAN_POINT('',(85.625,53.8155444566228,24.4)) ;
#18180 = CARTESIAN_POINT('Origin',(85.625,53.8155444566228,24.4)) ;
#18181 = CARTESIAN_POINT('',(85.625,53.8155444566228,25.8)) ;
#18182 = CARTESIAN_POINT('Origin',(85.7375,54.0104001724743,25.8)) ;
#18183 = CARTESIAN_POINT('Origin',(86.0195055291309,53.81293777516,25.8)) ;
#18184 = CARTESIAN_POINT('',(85.8748783169514,53.6405777754582,25.8)) ;
#18185 = CARTESIAN_POINT('',(85.8748783169514,53.6405777754582,25.8)) ;
#18186 = CARTESIAN_POINT('',(86.0415656304114,54.0881437924116,25.8)) ;
#18187 = CARTESIAN_POINT('Origin',(86.0415656304114,54.0881437924116,24.4)) ;
#18188 = CARTESIAN_POINT('',(85.8748783169514,53.6405777754582,24.4)) ;
#18189 = CARTESIAN_POINT('Origin',(85.8748783169514,53.6405777754582,24.4)) ;
#18190 = CARTESIAN_POINT('Origin',(86.3324517573119,53.8366998522094,24.4)) ;
#18191 = CARTESIAN_POINT('',(86.0905777754582,53.4248783169514,25.8)) ;
#18192 = CARTESIAN_POINT('',(86.3324517573119,53.8366998522094,25.8)) ;
#18193 = CARTESIAN_POINT('',(86.0905777754582,53.4248783169514,24.4)) ;
#18194 = CARTESIAN_POINT('Origin',(86.0905777754582,53.4248783169514,24.4)) ;
#18195 = CARTESIAN_POINT('',(86.0905777754582,53.4248783169514,25.8)) ;
#18196 = CARTESIAN_POINT('Origin',(86.26293777516,53.5695055291309,25.8)) ;
#18197 = CARTESIAN_POINT('Origin',(86.4604001724743,53.2875,25.8)) ;
#18198 = CARTESIAN_POINT('',(86.2655444566228,53.175,25.8)) ;
#18199 = CARTESIAN_POINT('',(86.2655444566228,53.175,25.8)) ;
#18200 = CARTESIAN_POINT('',(86.5752558883258,53.5385640646055,25.8)) ;
#18201 = CARTESIAN_POINT('Origin',(86.5752558883258,53.5385640646055,24.4)) ;
#18202 = CARTESIAN_POINT('',(86.2655444566228,53.175,24.4)) ;
#18203 = CARTESIAN_POINT('Origin',(86.2655444566228,53.175,24.4)) ;
#18204 = CARTESIAN_POINT('Origin',(86.7626005427969,53.2027951346422,24.4)) ;
#18205 = CARTESIAN_POINT('',(86.3944620863754,52.8985352508199,25.8)) ;
#18206 = CARTESIAN_POINT('',(86.7626005427969,53.2027951346422,25.8)) ;
#18207 = CARTESIAN_POINT('',(86.3944620863754,52.8985352508199,24.4)) ;
#18208 = CARTESIAN_POINT('Origin',(86.3944620863754,52.8985352508199,24.4)) ;
#18209 = CARTESIAN_POINT('',(86.3944620863754,52.8985352508199,25.8)) ;
#18210 = CARTESIAN_POINT('Origin',(86.6058929260522,52.9754897830682,25.8)) ;
#18211 = CARTESIAN_POINT('Origin',(86.6949953121991,52.6429551508922,25.8)) ;
#18212 = CARTESIAN_POINT('',(86.4734135677714,52.6038843109171,25.8)) ;
#18213 = CARTESIAN_POINT('',(86.4734135677714,52.6038843109171,25.8)) ;
#18214 = CARTESIAN_POINT('',(86.8887933482002,52.8395952313492,25.8)) ;
#18215 = CARTESIAN_POINT('Origin',(86.8887933482002,52.8395952313492,24.4)) ;
#18216 = CARTESIAN_POINT('',(86.4734135677714,52.6038843109171,24.4)) ;
#18217 = CARTESIAN_POINT('Origin',(86.4734135677714,52.6038843109171,24.4)) ;
#18218 = CARTESIAN_POINT('Origin',(86.95,52.46,24.4)) ;
#18219 = CARTESIAN_POINT('',(86.5,52.3,25.8)) ;
#18220 = CARTESIAN_POINT('',(86.95,52.46,25.8)) ;
#18221 = CARTESIAN_POINT('',(86.5,52.3,24.4)) ;
#18222 = CARTESIAN_POINT('Origin',(86.5,52.3,24.4)) ;
#18223 = CARTESIAN_POINT('',(86.5,52.3,25.8)) ;
#18224 = CARTESIAN_POINT('Origin',(86.725,52.3,25.8)) ;
#18225 = CARTESIAN_POINT('Origin',(84.75,52.3,26.2)) ;
#18226 = CARTESIAN_POINT('Origin',(83.05,52.3,26.2)) ;
#18227 = CARTESIAN_POINT('Origin',(84.75,52.3,24.4)) ;
#18228 = CARTESIAN_POINT('',(83.7339745962156,52.3,24.4)) ;
#18229 = CARTESIAN_POINT('Origin',(84.75,52.3,24.4)) ;
#18230 = CARTESIAN_POINT('Origin',(84.75,52.3,24.5)) ;
#18231 = CARTESIAN_POINT('',(83.8839745962156,52.3,24.55)) ;
#18232 = CARTESIAN_POINT('',(83.8339745962156,52.3,24.5)) ;
#18233 = CARTESIAN_POINT('',(83.9397035703159,52.2034745854044,24.6)) ;
#18234 = CARTESIAN_POINT('Ctrl Pts',(83.9397035703159,52.2034745854044,24.6)) ;
#18235 = CARTESIAN_POINT('Ctrl Pts',(83.9126673723676,52.2503026538944,24.5786927761521)) ;
#18236 = CARTESIAN_POINT('Ctrl Pts',(83.8839745962156,52.3,24.55)) ;
#18237 = CARTESIAN_POINT('',(84.2612583240074,51.6465254145956,24.6)) ;
#18238 = CARTESIAN_POINT('Origin',(84.75,52.3,24.6)) ;
#18239 = CARTESIAN_POINT('',(84.3169872981078,51.55,24.55)) ;
#18240 = CARTESIAN_POINT('Ctrl Pts',(84.3169872981078,51.55,24.55)) ;
#18241 = CARTESIAN_POINT('Ctrl Pts',(84.2882945219557,51.5996973461057,24.5786927761521)) ;
#18242 = CARTESIAN_POINT('Ctrl Pts',(84.2612583240074,51.6465254145956,24.6)) ;
#18243 = CARTESIAN_POINT('',(84.4284452463086,51.55,24.6)) ;
#18244 = CARTESIAN_POINT('Ctrl Pts',(84.4284452463086,51.55,24.6)) ;
#18245 = CARTESIAN_POINT('Ctrl Pts',(84.374372850412,51.55,24.5786927761522)) ;
#18246 = CARTESIAN_POINT('Ctrl Pts',(84.3169872981078,51.55,24.55)) ;
#18247 = CARTESIAN_POINT('',(85.0715547536914,51.55,24.6)) ;
#18248 = CARTESIAN_POINT('Origin',(84.75,52.3,24.6)) ;
#18249 = CARTESIAN_POINT('',(85.1830127018922,51.55,24.55)) ;
#18250 = CARTESIAN_POINT('Ctrl Pts',(85.1830127018922,51.55,24.55)) ;
#18251 = CARTESIAN_POINT('Ctrl Pts',(85.125627149588,51.55,24.5786927761521)) ;
#18252 = CARTESIAN_POINT('Ctrl Pts',(85.0715547536914,51.55,24.6)) ;
#18253 = CARTESIAN_POINT('',(85.2387416759926,51.6465254145956,24.6)) ;
#18254 = CARTESIAN_POINT('Ctrl Pts',(85.2387416759926,51.6465254145956,24.6)) ;
#18255 = CARTESIAN_POINT('Ctrl Pts',(85.2117054780443,51.5996973461057,24.5786927761521)) ;
#18256 = CARTESIAN_POINT('Ctrl Pts',(85.1830127018922,51.55,24.55)) ;
#18257 = CARTESIAN_POINT('',(85.560296429684,52.2034745854045,24.6)) ;
#18258 = CARTESIAN_POINT('Origin',(84.75,52.3,24.6)) ;
#18259 = CARTESIAN_POINT('',(85.6160254037844,52.3,24.55)) ;
#18260 = CARTESIAN_POINT('Ctrl Pts',(85.6160254037844,52.3,24.55)) ;
#18261 = CARTESIAN_POINT('Ctrl Pts',(85.5873326276323,52.2503026538944,24.5786927761521)) ;
#18262 = CARTESIAN_POINT('Ctrl Pts',(85.5602964296841,52.2034745854045,24.6)) ;
#18263 = CARTESIAN_POINT('',(85.560296429684,52.3965254145956,24.6)) ;
#18264 = CARTESIAN_POINT('Ctrl Pts',(85.560296429684,52.3965254145956,24.6)) ;
#18265 = CARTESIAN_POINT('Ctrl Pts',(85.5873326276323,52.3496973461056,24.5786927761521)) ;
#18266 = CARTESIAN_POINT('Ctrl Pts',(85.6160254037844,52.3,24.55)) ;
#18267 = CARTESIAN_POINT('',(85.2387416759926,52.9534745854044,24.6)) ;
#18268 = CARTESIAN_POINT('Origin',(84.75,52.3,24.6)) ;
#18269 = CARTESIAN_POINT('',(85.1830127018922,53.05,24.55)) ;
#18270 = CARTESIAN_POINT('Ctrl Pts',(85.1830127018922,53.05,24.55)) ;
#18271 = CARTESIAN_POINT('Ctrl Pts',(85.2117054780443,53.0003026538944,24.5786927761521)) ;
#18272 = CARTESIAN_POINT('Ctrl Pts',(85.2387416759926,52.9534745854044,24.6)) ;
#18273 = CARTESIAN_POINT('',(85.0715547536915,53.05,24.6)) ;
#18274 = CARTESIAN_POINT('Ctrl Pts',(85.0715547536915,53.05,24.6)) ;
#18275 = CARTESIAN_POINT('Ctrl Pts',(85.125627149588,53.05,24.5786927761521)) ;
#18276 = CARTESIAN_POINT('Ctrl Pts',(85.1830127018922,53.05,24.55)) ;
#18277 = CARTESIAN_POINT('',(84.4284452463085,53.05,24.6)) ;
#18278 = CARTESIAN_POINT('Origin',(84.75,52.3,24.6)) ;
#18279 = CARTESIAN_POINT('',(84.3169872981078,53.05,24.55)) ;
#18280 = CARTESIAN_POINT('Ctrl Pts',(84.3169872981078,53.05,24.55)) ;
#18281 = CARTESIAN_POINT('Ctrl Pts',(84.374372850412,53.05,24.5786927761522)) ;
#18282 = CARTESIAN_POINT('Ctrl Pts',(84.4284452463085,53.05,24.6)) ;
#18283 = CARTESIAN_POINT('',(84.2612583240074,52.9534745854045,24.6)) ;
#18284 = CARTESIAN_POINT('Ctrl Pts',(84.2612583240074,52.9534745854045,24.6)) ;
#18285 = CARTESIAN_POINT('Ctrl Pts',(84.2882945219557,53.0003026538944,24.5786927761521)) ;
#18286 = CARTESIAN_POINT('Ctrl Pts',(84.3169872981078,53.05,24.55)) ;
#18287 = CARTESIAN_POINT('',(83.9397035703159,52.3965254145955,24.6)) ;
#18288 = CARTESIAN_POINT('Origin',(84.75,52.3,24.6)) ;
#18289 = CARTESIAN_POINT('Ctrl Pts',(83.8839745962156,52.3,24.55)) ;
#18290 = CARTESIAN_POINT('Ctrl Pts',(83.9126673723676,52.3496973461056,24.5786927761521)) ;
#18291 = CARTESIAN_POINT('Ctrl Pts',(83.9397035703159,52.3965254145955,24.6)) ;
#18292 = CARTESIAN_POINT('Origin',(84.75,52.3,24.5)) ;
#18293 = CARTESIAN_POINT('',(85.560296429684,52.2034745854045,24.4)) ;
#18294 = CARTESIAN_POINT('',(85.560296429684,52.2034745854045,24.5)) ;
#18295 = CARTESIAN_POINT('',(85.2387416759926,51.6465254145956,24.4)) ;
#18296 = CARTESIAN_POINT('',(85.2387416759926,51.6465254145956,24.5)) ;
#18297 = CARTESIAN_POINT('Origin',(84.75,52.3,24.4)) ;
#18298 = CARTESIAN_POINT('Origin',(84.75,52.3,24.5)) ;
#18299 = CARTESIAN_POINT('',(85.2387416759926,52.9534745854044,24.4)) ;
#18300 = CARTESIAN_POINT('',(85.2387416759926,52.9534745854044,24.5)) ;
#18301 = CARTESIAN_POINT('',(85.560296429684,52.3965254145956,24.4)) ;
#18302 = CARTESIAN_POINT('',(85.560296429684,52.3965254145956,24.5)) ;
#18303 = CARTESIAN_POINT('Origin',(84.75,52.3,24.4)) ;
#18304 = CARTESIAN_POINT('Origin',(84.75,52.3,24.5)) ;
#18305 = CARTESIAN_POINT('',(84.4284452463086,51.55,24.4)) ;
#18306 = CARTESIAN_POINT('',(84.4284452463086,51.55,24.5)) ;
#18307 = CARTESIAN_POINT('',(85.0715547536914,51.55,24.4)) ;
#18308 = CARTESIAN_POINT('Origin',(84.75,52.3,24.4)) ;
#18309 = CARTESIAN_POINT('',(85.0715547536914,51.55,24.5)) ;
#18310 = CARTESIAN_POINT('Origin',(84.75,52.3,24.5)) ;
#18311 = CARTESIAN_POINT('',(84.4284452463085,53.05,24.4)) ;
#18312 = CARTESIAN_POINT('',(84.4284452463085,53.05,24.5)) ;
#18313 = CARTESIAN_POINT('',(85.0715547536915,53.05,24.4)) ;
#18314 = CARTESIAN_POINT('',(85.0715547536915,53.05,24.5)) ;
#18315 = CARTESIAN_POINT('Origin',(84.75,52.3,24.4)) ;
#18316 = CARTESIAN_POINT('Origin',(84.75,52.3,24.5)) ;
#18317 = CARTESIAN_POINT('',(83.9397035703159,52.2034745854044,24.4)) ;
#18318 = CARTESIAN_POINT('',(83.9397035703159,52.2034745854044,24.5)) ;
#18319 = CARTESIAN_POINT('',(84.2612583240074,51.6465254145956,24.4)) ;
#18320 = CARTESIAN_POINT('Origin',(84.75,52.3,24.4)) ;
#18321 = CARTESIAN_POINT('',(84.2612583240074,51.6465254145956,24.5)) ;
#18322 = CARTESIAN_POINT('Origin',(84.75,52.3,24.5)) ;
#18323 = CARTESIAN_POINT('',(84.2612583240074,52.9534745854045,24.4)) ;
#18324 = CARTESIAN_POINT('',(84.2612583240074,52.9534745854045,24.5)) ;
#18325 = CARTESIAN_POINT('',(83.9397035703159,52.3965254145955,24.4)) ;
#18326 = CARTESIAN_POINT('Origin',(84.75,52.3,24.4)) ;
#18327 = CARTESIAN_POINT('',(83.9397035703159,52.3965254145955,24.5)) ;
#18328 = CARTESIAN_POINT('Origin',(85.1830127018922,53.05,24.4)) ;
#18329 = CARTESIAN_POINT('',(84.9665063509461,53.05,24.4)) ;
#18330 = CARTESIAN_POINT('',(85.1830127018922,53.05,25.4)) ;
#18331 = CARTESIAN_POINT('',(85.1830127018922,53.05,24.4)) ;
#18332 = CARTESIAN_POINT('',(84.3169872981078,53.05,25.4)) ;
#18333 = CARTESIAN_POINT('',(85.1830127018922,53.05,25.4)) ;
#18334 = CARTESIAN_POINT('',(84.3169872981078,53.05,24.4)) ;
#18335 = CARTESIAN_POINT('Origin',(85.6160254037844,52.3,24.4)) ;
#18336 = CARTESIAN_POINT('',(85.5077722283114,52.4875,24.4)) ;
#18337 = CARTESIAN_POINT('',(85.6160254037844,52.3,25.4)) ;
#18338 = CARTESIAN_POINT('',(85.6160254037844,52.3,24.4)) ;
#18339 = CARTESIAN_POINT('',(85.6160254037844,52.3,25.4)) ;
#18340 = CARTESIAN_POINT('Origin',(85.1830127018922,51.55,24.4)) ;
#18341 = CARTESIAN_POINT('',(85.2912658773653,51.7375,24.4)) ;
#18342 = CARTESIAN_POINT('',(85.1830127018922,51.55,25.4)) ;
#18343 = CARTESIAN_POINT('',(85.1830127018922,51.55,24.4)) ;
#18344 = CARTESIAN_POINT('',(85.1830127018922,51.55,25.4)) ;
#18345 = CARTESIAN_POINT('Origin',(84.75,52.3,24.4)) ;
#18346 = CARTESIAN_POINT('Origin',(84.75,52.3,24.4)) ;
#18347 = CARTESIAN_POINT('Origin',(84.75,52.3,24.4)) ;
#18348 = CARTESIAN_POINT('',(84.5334936490539,51.55,24.4)) ;
#18349 = CARTESIAN_POINT('Origin',(84.75,52.3,24.4)) ;
#18350 = CARTESIAN_POINT('Origin',(84.75,52.3,24.4)) ;
#18351 = CARTESIAN_POINT('',(83.9922277716886,52.1125,24.4)) ;
#18352 = CARTESIAN_POINT('Origin',(84.75,52.3,24.4)) ;
#18353 = CARTESIAN_POINT('',(84.2087341226347,52.8625,24.4)) ;
#18354 = CARTESIAN_POINT('Origin',(85.6160254037844,52.3,25.4)) ;
#18355 = CARTESIAN_POINT('',(84.3169872981078,51.55,25.4)) ;
#18356 = CARTESIAN_POINT('',(84.3169872981078,51.55,25.4)) ;
#18357 = CARTESIAN_POINT('Origin',(84.75,52.3,25.4)) ;
#18358 = CARTESIAN_POINT('Origin',(85.6160254037844,52.3,25.4)) ;
#18359 = CARTESIAN_POINT('Origin',(84.75,52.3,25.4)) ;
#18360 = CARTESIAN_POINT('Origin',(85.6160254037844,52.3,25.4)) ;
#18361 = CARTESIAN_POINT('Origin',(84.75,52.3,25.4)) ;
#18362 = CARTESIAN_POINT('Origin',(85.6160254037844,52.3,25.4)) ;
#18363 = CARTESIAN_POINT('Origin',(84.75,52.3,25.4)) ;
#18364 = CARTESIAN_POINT('Origin',(85.6160254037844,52.3,25.4)) ;
#18365 = CARTESIAN_POINT('',(83.8839745962156,52.3,25.4)) ;
#18366 = CARTESIAN_POINT('',(84.3169872981078,53.05,25.4)) ;
#18367 = CARTESIAN_POINT('Origin',(84.75,52.3,25.4)) ;
#18368 = CARTESIAN_POINT('Origin',(85.6160254037844,52.3,25.4)) ;
#18369 = CARTESIAN_POINT('',(83.8839745962156,52.3,25.4)) ;
#18370 = CARTESIAN_POINT('Origin',(84.75,52.3,25.4)) ;
#18371 = CARTESIAN_POINT('Origin',(84.75,52.3,25.4)) ;
#18372 = CARTESIAN_POINT('',(84.75,52.3,25.9203605602115)) ;
#18373 = CARTESIAN_POINT('',(83.8839745962156,52.3,25.4)) ;
#18374 = CARTESIAN_POINT('Origin',(84.3169872981078,51.55,24.4)) ;
#18375 = CARTESIAN_POINT('',(84.3169872981078,51.55,24.4)) ;
#18376 = CARTESIAN_POINT('Origin',(83.8839745962156,52.3,24.4)) ;
#18377 = CARTESIAN_POINT('',(83.8839745962156,52.3,24.4)) ;
#18378 = CARTESIAN_POINT('Origin',(84.3169872981078,53.05,24.4)) ;
#18379 = CARTESIAN_POINT('',(0.,0.,0.)) ;
#18380 = CARTESIAN_POINT('Origin',(84.75,52.3,27.6)) ;
#18381 = CARTESIAN_POINT('',(83.6,52.3,27.6)) ;
#18382 = CARTESIAN_POINT('Origin',(84.75,52.3,27.6)) ;
#18383 = CARTESIAN_POINT('',(83.6,52.3,26.4)) ;
#18384 = CARTESIAN_POINT('',(83.6,52.3,27.6)) ;
#18385 = CARTESIAN_POINT('Origin',(84.75,52.3,26.4)) ;
#18386 = CARTESIAN_POINT('Origin',(71.75,52.3,27.6)) ;
#18387 = CARTESIAN_POINT('',(70.6,52.3,27.6)) ;
#18388 = CARTESIAN_POINT('Origin',(71.75,52.3,27.6)) ;
#18389 = CARTESIAN_POINT('',(70.6,52.3,26.4)) ;
#18390 = CARTESIAN_POINT('',(70.6,52.3,27.6)) ;
#18391 = CARTESIAN_POINT('Origin',(71.75,52.3,26.4)) ;
#18392 = CARTESIAN_POINT('Origin',(73.25,47.15,24.9)) ;
#18393 = CARTESIAN_POINT('',(76.311572802502,48.35,24.9)) ;
#18394 = CARTESIAN_POINT('',(80.188427197498,48.35,24.9)) ;
#18395 = CARTESIAN_POINT('Origin',(78.25,52.3,24.9)) ;
#18396 = CARTESIAN_POINT('',(73.25,48.35,24.9)) ;
#18397 = CARTESIAN_POINT('',(73.25,48.35,24.9)) ;
#18398 = CARTESIAN_POINT('',(73.25,47.15,24.9)) ;
#18399 = CARTESIAN_POINT('',(73.25,47.15,24.9)) ;
#18400 = CARTESIAN_POINT('',(83.25,47.15,24.9)) ;
#18401 = CARTESIAN_POINT('',(73.25,47.15,24.9)) ;
#18402 = CARTESIAN_POINT('',(83.25,48.35,24.9)) ;
#18403 = CARTESIAN_POINT('',(83.25,47.15,24.9)) ;
#18404 = CARTESIAN_POINT('',(73.25,48.35,24.9)) ;
#18405 = CARTESIAN_POINT('Origin',(78.25,47.15,11.65)) ;
#18406 = CARTESIAN_POINT('',(76.2,48.35,11.65)) ;
#18407 = CARTESIAN_POINT('Origin',(78.25,48.35,11.65)) ;
#18408 = CARTESIAN_POINT('',(76.2,47.15,11.65)) ;
#18409 = CARTESIAN_POINT('',(76.2,47.15,11.65)) ;
#18410 = CARTESIAN_POINT('Origin',(78.25,47.15,11.65)) ;
#18411 = CARTESIAN_POINT('Origin',(73.25,47.15,11.65)) ;
#18412 = CARTESIAN_POINT('',(73.25,47.15,11.65)) ;
#18413 = CARTESIAN_POINT('',(73.25,47.15,11.65)) ;
#18414 = CARTESIAN_POINT('',(73.25,48.35,11.65)) ;
#18415 = CARTESIAN_POINT('',(73.25,48.35,11.65)) ;
#18416 = CARTESIAN_POINT('',(73.25,47.15,11.65)) ;
#18417 = CARTESIAN_POINT('Origin',(78.25,47.15,11.65)) ;
#18418 = CARTESIAN_POINT('',(83.25,47.15,11.65)) ;
#18419 = CARTESIAN_POINT('Origin',(78.25,47.15,11.65)) ;
#18420 = CARTESIAN_POINT('',(83.25,48.35,11.65)) ;
#18421 = CARTESIAN_POINT('Origin',(78.25,48.35,11.65)) ;
#18422 = CARTESIAN_POINT('',(83.25,47.15,11.65)) ;
#18423 = CARTESIAN_POINT('Origin',(83.25,47.15,24.9)) ;
#18424 = CARTESIAN_POINT('',(83.25,47.15,24.9)) ;
#18425 = CARTESIAN_POINT('',(83.25,48.35,24.9)) ;
#18426 = CARTESIAN_POINT('Origin',(78.25,48.35,15.775)) ;
#18427 = CARTESIAN_POINT('',(80.188427197498,48.35,24.4)) ;
#18428 = CARTESIAN_POINT('',(80.188427197498,48.35,25.4)) ;
#18429 = CARTESIAN_POINT('',(76.311572802502,48.35,24.4)) ;
#18430 = CARTESIAN_POINT('',(76.311572802502,48.35,25.4)) ;
#18431 = CARTESIAN_POINT('',(80.45,48.35,24.4)) ;
#18432 = CARTESIAN_POINT('Origin',(78.25,47.15,15.775)) ;
#18433 = CARTESIAN_POINT('Origin',(82.65,52.3,24.4)) ;
#18434 = CARTESIAN_POINT('',(73.85,52.3,24.4)) ;
#18435 = CARTESIAN_POINT('Origin',(78.25,52.3,24.4)) ;
#18436 = CARTESIAN_POINT('',(76.311572802502,56.25,24.4)) ;
#18437 = CARTESIAN_POINT('Origin',(78.25,52.3,24.4)) ;
#18438 = CARTESIAN_POINT('',(80.188427197498,56.25,24.4)) ;
#18439 = CARTESIAN_POINT('',(80.45,56.25,24.4)) ;
#18440 = CARTESIAN_POINT('Origin',(78.25,52.3,24.4)) ;
#18441 = CARTESIAN_POINT('Origin',(78.25,56.25,15.775)) ;
#18442 = CARTESIAN_POINT('',(80.188427197498,56.25,24.9)) ;
#18443 = CARTESIAN_POINT('',(80.188427197498,56.25,25.4)) ;
#18444 = CARTESIAN_POINT('',(76.311572802502,56.25,24.9)) ;
#18445 = CARTESIAN_POINT('',(76.311572802502,56.25,25.4)) ;
#18446 = CARTESIAN_POINT('',(73.25,56.25,24.9)) ;
#18447 = CARTESIAN_POINT('',(73.25,56.25,24.9)) ;
#18448 = CARTESIAN_POINT('',(73.25,56.25,11.65)) ;
#18449 = CARTESIAN_POINT('',(73.25,56.25,11.65)) ;
#18450 = CARTESIAN_POINT('',(83.25,56.25,11.65)) ;
#18451 = CARTESIAN_POINT('Origin',(78.25,56.25,11.65)) ;
#18452 = CARTESIAN_POINT('',(83.25,56.25,24.9)) ;
#18453 = CARTESIAN_POINT('',(83.25,56.25,24.9)) ;
#18454 = CARTESIAN_POINT('',(73.25,56.25,24.9)) ;
#18455 = CARTESIAN_POINT('',(76.2,56.25,11.65)) ;
#18456 = CARTESIAN_POINT('Origin',(78.25,56.25,11.65)) ;
#18457 = CARTESIAN_POINT('Origin',(78.25,56.25,11.65)) ;
#18458 = CARTESIAN_POINT('',(76.2,57.45,11.65)) ;
#18459 = CARTESIAN_POINT('Origin',(78.25,57.45,11.65)) ;
#18460 = CARTESIAN_POINT('',(76.2,56.25,11.65)) ;
#18461 = CARTESIAN_POINT('Origin',(73.25,56.25,11.65)) ;
#18462 = CARTESIAN_POINT('',(73.25,57.45,24.9)) ;
#18463 = CARTESIAN_POINT('',(73.25,56.25,24.9)) ;
#18464 = CARTESIAN_POINT('',(73.25,57.45,11.65)) ;
#18465 = CARTESIAN_POINT('',(73.25,57.45,11.65)) ;
#18466 = CARTESIAN_POINT('',(73.25,56.25,11.65)) ;
#18467 = CARTESIAN_POINT('Origin',(78.25,56.25,11.65)) ;
#18468 = CARTESIAN_POINT('',(83.25,57.45,11.65)) ;
#18469 = CARTESIAN_POINT('Origin',(78.25,57.45,11.65)) ;
#18470 = CARTESIAN_POINT('',(83.25,56.25,11.65)) ;
#18471 = CARTESIAN_POINT('Origin',(83.25,56.25,24.9)) ;
#18472 = CARTESIAN_POINT('',(83.25,57.45,24.9)) ;
#18473 = CARTESIAN_POINT('',(83.25,57.45,24.9)) ;
#18474 = CARTESIAN_POINT('',(83.25,56.25,24.9)) ;
#18475 = CARTESIAN_POINT('Origin',(73.25,56.25,24.9)) ;
#18476 = CARTESIAN_POINT('Origin',(78.25,52.3,24.9)) ;
#18477 = CARTESIAN_POINT('',(73.25,57.45,24.9)) ;
#18478 = CARTESIAN_POINT('Origin',(78.25,57.45,15.775)) ;
#18479 = CARTESIAN_POINT('Origin',(78.25,52.3,25.4)) ;
#18480 = CARTESIAN_POINT('',(73.85,52.3,26.4)) ;
#18481 = CARTESIAN_POINT('Origin',(78.25,52.3,26.4)) ;
#18482 = CARTESIAN_POINT('',(73.85,52.3,25.4)) ;
#18483 = CARTESIAN_POINT('Origin',(79.75,52.3,26.)) ;
#18484 = CARTESIAN_POINT('',(76.75,52.3,26.)) ;
#18485 = CARTESIAN_POINT('Origin',(78.25,52.3,26.)) ;
#18486 = CARTESIAN_POINT('Origin',(78.25,52.3,27.)) ;
#18487 = CARTESIAN_POINT('',(76.75,52.3,27.6)) ;
#18488 = CARTESIAN_POINT('',(76.75,52.3,27.)) ;
#18489 = CARTESIAN_POINT('Origin',(78.25,52.3,27.6)) ;
#18490 = CARTESIAN_POINT('Origin',(87.25,59.3,26.4)) ;
#18491 = CARTESIAN_POINT('',(87.25,59.3,26.4)) ;
#18492 = CARTESIAN_POINT('',(69.25,59.3,26.4)) ;
#18493 = CARTESIAN_POINT('',(87.25,59.3,26.4)) ;
#18494 = CARTESIAN_POINT('',(69.25,59.3,27.6)) ;
#18495 = CARTESIAN_POINT('',(69.25,59.3,26.4)) ;
#18496 = CARTESIAN_POINT('',(87.25,59.3,27.6)) ;
#18497 = CARTESIAN_POINT('',(87.25,59.3,27.6)) ;
#18498 = CARTESIAN_POINT('',(87.25,59.3,26.4)) ;
#18499 = CARTESIAN_POINT('Origin',(87.25,45.3,26.4)) ;
#18500 = CARTESIAN_POINT('',(87.25,45.3,26.4)) ;
#18501 = CARTESIAN_POINT('',(87.25,45.3,26.4)) ;
#18502 = CARTESIAN_POINT('',(87.25,45.3,27.6)) ;
#18503 = CARTESIAN_POINT('',(87.25,45.3,27.6)) ;
#18504 = CARTESIAN_POINT('',(87.25,45.3,26.4)) ;
#18505 = CARTESIAN_POINT('Origin',(69.25,45.3,26.4)) ;
#18506 = CARTESIAN_POINT('',(69.25,45.3,26.4)) ;
#18507 = CARTESIAN_POINT('',(69.25,45.3,26.4)) ;
#18508 = CARTESIAN_POINT('',(69.25,45.3,27.6)) ;
#18509 = CARTESIAN_POINT('',(69.25,45.3,27.6)) ;
#18510 = CARTESIAN_POINT('',(69.25,45.3,26.4)) ;
#18511 = CARTESIAN_POINT('Origin',(69.25,59.3,26.4)) ;
#18512 = CARTESIAN_POINT('',(69.25,59.3,26.4)) ;
#18513 = CARTESIAN_POINT('',(69.25,59.3,27.6)) ;
#18514 = CARTESIAN_POINT('Origin',(78.25,52.3,27.6)) ;
#18515 = CARTESIAN_POINT('Origin',(78.25,52.3,26.4)) ;
#18516 = CARTESIAN_POINT('',(0.,0.,0.)) ;
#18517 = CARTESIAN_POINT('Origin',(-71.75,52.3,27.6)) ;
#18518 = CARTESIAN_POINT('',(-72.9,52.3,27.6)) ;
#18519 = CARTESIAN_POINT('Origin',(-71.75,52.3,27.6)) ;
#18520 = CARTESIAN_POINT('',(-72.9,52.3,26.4)) ;
#18521 = CARTESIAN_POINT('',(-72.9,52.3,27.6)) ;
#18522 = CARTESIAN_POINT('Origin',(-71.75,52.3,26.4)) ;
#18523 = CARTESIAN_POINT('Origin',(-84.75,52.3,27.6)) ;
#18524 = CARTESIAN_POINT('',(-85.9,52.3,27.6)) ;
#18525 = CARTESIAN_POINT('Origin',(-84.75,52.3,27.6)) ;
#18526 = CARTESIAN_POINT('',(-85.9,52.3,26.4)) ;
#18527 = CARTESIAN_POINT('',(-85.9,52.3,27.6)) ;
#18528 = CARTESIAN_POINT('Origin',(-84.75,52.3,26.4)) ;
#18529 = CARTESIAN_POINT('Origin',(-78.25,48.35,16.775)) ;
#18530 = CARTESIAN_POINT('',(-73.25,48.35,26.4)) ;
#18531 = CARTESIAN_POINT('',(-83.25,48.35,26.4)) ;
#18532 = CARTESIAN_POINT('',(-78.25,48.35,26.4)) ;
#18533 = CARTESIAN_POINT('',(-73.25,48.35,11.65)) ;
#18534 = CARTESIAN_POINT('',(-73.25,48.35,26.9)) ;
#18535 = CARTESIAN_POINT('',(-83.25,48.35,11.65)) ;
#18536 = CARTESIAN_POINT('Origin',(-78.25,48.35,11.65)) ;
#18537 = CARTESIAN_POINT('',(-83.25,48.35,11.65)) ;
#18538 = CARTESIAN_POINT('',(-80.3,48.35,11.65)) ;
#18539 = CARTESIAN_POINT('Origin',(-78.25,48.35,11.65)) ;
#18540 = CARTESIAN_POINT('Origin',(-73.25,47.15,26.9)) ;
#18541 = CARTESIAN_POINT('',(-73.25,47.15,26.4)) ;
#18542 = CARTESIAN_POINT('',(-73.25,49.725,26.4)) ;
#18543 = CARTESIAN_POINT('',(-73.25,47.15,11.65)) ;
#18544 = CARTESIAN_POINT('',(-73.25,47.15,26.9)) ;
#18545 = CARTESIAN_POINT('',(-73.25,47.15,11.65)) ;
#18546 = CARTESIAN_POINT('Origin',(-78.25,47.15,11.65)) ;
#18547 = CARTESIAN_POINT('',(-80.3,47.15,11.65)) ;
#18548 = CARTESIAN_POINT('',(-80.3,47.15,11.65)) ;
#18549 = CARTESIAN_POINT('Origin',(-78.25,47.15,11.65)) ;
#18550 = CARTESIAN_POINT('Origin',(-83.25,47.15,11.65)) ;
#18551 = CARTESIAN_POINT('',(-83.25,47.15,26.4)) ;
#18552 = CARTESIAN_POINT('',(-83.25,49.725,26.4)) ;
#18553 = CARTESIAN_POINT('',(-83.25,47.15,11.65)) ;
#18554 = CARTESIAN_POINT('',(-83.25,47.15,11.65)) ;
#18555 = CARTESIAN_POINT('',(-83.25,47.15,11.65)) ;
#18556 = CARTESIAN_POINT('Origin',(-78.25,47.15,11.65)) ;
#18557 = CARTESIAN_POINT('Origin',(-78.25,47.15,11.65)) ;
#18558 = CARTESIAN_POINT('Origin',(-78.25,47.15,16.775)) ;
#18559 = CARTESIAN_POINT('',(-78.25,47.15,26.4)) ;
#18560 = CARTESIAN_POINT('Origin',(-78.25,57.45,16.775)) ;
#18561 = CARTESIAN_POINT('',(-73.25,57.45,26.4)) ;
#18562 = CARTESIAN_POINT('',(-83.25,57.45,26.4)) ;
#18563 = CARTESIAN_POINT('',(-78.25,57.45,26.4)) ;
#18564 = CARTESIAN_POINT('',(-73.25,57.45,11.65)) ;
#18565 = CARTESIAN_POINT('',(-73.25,57.45,26.9)) ;
#18566 = CARTESIAN_POINT('',(-83.25,57.45,11.65)) ;
#18567 = CARTESIAN_POINT('Origin',(-78.25,57.45,11.65)) ;
#18568 = CARTESIAN_POINT('',(-83.25,57.45,11.65)) ;
#18569 = CARTESIAN_POINT('',(-80.3,57.45,11.65)) ;
#18570 = CARTESIAN_POINT('Origin',(-78.25,57.45,11.65)) ;
#18571 = CARTESIAN_POINT('Origin',(-73.25,56.25,26.9)) ;
#18572 = CARTESIAN_POINT('',(-73.25,56.25,26.4)) ;
#18573 = CARTESIAN_POINT('',(-73.25,54.275,26.4)) ;
#18574 = CARTESIAN_POINT('',(-73.25,56.25,11.65)) ;
#18575 = CARTESIAN_POINT('',(-73.25,56.25,26.9)) ;
#18576 = CARTESIAN_POINT('',(-73.25,56.25,11.65)) ;
#18577 = CARTESIAN_POINT('Origin',(-78.25,56.25,11.65)) ;
#18578 = CARTESIAN_POINT('',(-80.3,56.25,11.65)) ;
#18579 = CARTESIAN_POINT('',(-80.3,56.25,11.65)) ;
#18580 = CARTESIAN_POINT('Origin',(-78.25,56.25,11.65)) ;
#18581 = CARTESIAN_POINT('Origin',(-83.25,56.25,11.65)) ;
#18582 = CARTESIAN_POINT('',(-83.25,56.25,26.4)) ;
#18583 = CARTESIAN_POINT('',(-83.25,54.275,26.4)) ;
#18584 = CARTESIAN_POINT('',(-83.25,56.25,11.65)) ;
#18585 = CARTESIAN_POINT('',(-83.25,56.25,11.65)) ;
#18586 = CARTESIAN_POINT('',(-83.25,56.25,11.65)) ;
#18587 = CARTESIAN_POINT('Origin',(-78.25,56.25,11.65)) ;
#18588 = CARTESIAN_POINT('Origin',(-78.25,56.25,11.65)) ;
#18589 = CARTESIAN_POINT('Origin',(-78.25,56.25,16.775)) ;
#18590 = CARTESIAN_POINT('',(-78.25,56.25,26.4)) ;
#18591 = CARTESIAN_POINT('Origin',(-69.25,59.3,26.4)) ;
#18592 = CARTESIAN_POINT('',(-69.25,59.3,26.4)) ;
#18593 = CARTESIAN_POINT('',(-87.25,59.3,26.4)) ;
#18594 = CARTESIAN_POINT('',(-69.25,59.3,26.4)) ;
#18595 = CARTESIAN_POINT('',(-87.25,59.3,27.6)) ;
#18596 = CARTESIAN_POINT('',(-87.25,59.3,26.4)) ;
#18597 = CARTESIAN_POINT('',(-69.25,59.3,27.6)) ;
#18598 = CARTESIAN_POINT('',(-69.25,59.3,27.6)) ;
#18599 = CARTESIAN_POINT('',(-69.25,59.3,26.4)) ;
#18600 = CARTESIAN_POINT('Origin',(-69.25,45.3,26.4)) ;
#18601 = CARTESIAN_POINT('',(-69.25,45.3,26.4)) ;
#18602 = CARTESIAN_POINT('',(-69.25,45.3,26.4)) ;
#18603 = CARTESIAN_POINT('',(-69.25,45.3,27.6)) ;
#18604 = CARTESIAN_POINT('',(-69.25,45.3,27.6)) ;
#18605 = CARTESIAN_POINT('',(-69.25,45.3,26.4)) ;
#18606 = CARTESIAN_POINT('Origin',(-87.25,45.3,26.4)) ;
#18607 = CARTESIAN_POINT('',(-87.25,45.3,26.4)) ;
#18608 = CARTESIAN_POINT('',(-87.25,45.3,26.4)) ;
#18609 = CARTESIAN_POINT('',(-87.25,45.3,27.6)) ;
#18610 = CARTESIAN_POINT('',(-87.25,45.3,27.6)) ;
#18611 = CARTESIAN_POINT('',(-87.25,45.3,26.4)) ;
#18612 = CARTESIAN_POINT('Origin',(-87.25,59.3,26.4)) ;
#18613 = CARTESIAN_POINT('',(-87.25,59.3,26.4)) ;
#18614 = CARTESIAN_POINT('',(-87.25,59.3,27.6)) ;
#18615 = CARTESIAN_POINT('Origin',(-78.25,52.3,27.6)) ;
#18616 = CARTESIAN_POINT('Origin',(-78.25,52.3,26.4)) ;
#18617 = CARTESIAN_POINT('',(0.,0.,0.)) ;
#18618 = CARTESIAN_POINT('Origin',(84.25,55.95,11.65)) ;
#18619 = CARTESIAN_POINT('',(72.25,55.95,11.65)) ;
#18620 = CARTESIAN_POINT('Origin',(78.25,55.95,11.65)) ;
#18621 = CARTESIAN_POINT('',(76.2,55.95,11.65)) ;
#18622 = CARTESIAN_POINT('Origin',(78.25,55.95,11.65)) ;
#18623 = CARTESIAN_POINT('Origin',(78.25,55.45,11.65)) ;
#18624 = CARTESIAN_POINT('',(72.25,54.95,11.65)) ;
#18625 = CARTESIAN_POINT('Origin',(78.25,54.95,11.65)) ;
#18626 = CARTESIAN_POINT('',(72.25,55.45,11.65)) ;
#18627 = CARTESIAN_POINT('Origin',(87.9,54.95,11.65)) ;
#18628 = CARTESIAN_POINT('',(68.6,54.95,11.65)) ;
#18629 = CARTESIAN_POINT('Origin',(78.25,54.95,11.65)) ;
#18630 = CARTESIAN_POINT('Origin',(78.25,54.65,11.65)) ;
#18631 = CARTESIAN_POINT('',(67.2,54.35,11.65)) ;
#18632 = CARTESIAN_POINT('Origin',(78.25,54.35,11.65)) ;
#18633 = CARTESIAN_POINT('',(67.9,54.65,11.65)) ;
#18634 = CARTESIAN_POINT('Origin',(78.25,54.075,11.65)) ;
#18635 = CARTESIAN_POINT('',(66.6,53.8,11.65)) ;
#18636 = CARTESIAN_POINT('Origin',(78.25,53.8,11.65)) ;
#18637 = CARTESIAN_POINT('',(66.9,54.075,11.65)) ;
#18638 = CARTESIAN_POINT('Origin',(78.25,52.3,11.65)) ;
#18639 = CARTESIAN_POINT('',(66.6,50.8,11.65)) ;
#18640 = CARTESIAN_POINT('Origin',(78.25,50.8,11.65)) ;
#18641 = CARTESIAN_POINT('',(66.6,52.3,11.65)) ;
#18642 = CARTESIAN_POINT('Origin',(78.25,50.525,11.65)) ;
#18643 = CARTESIAN_POINT('',(67.2,50.25,11.65)) ;
#18644 = CARTESIAN_POINT('Origin',(78.25,50.25,11.65)) ;
#18645 = CARTESIAN_POINT('',(66.9,50.525,11.65)) ;
#18646 = CARTESIAN_POINT('Origin',(78.25,49.95,11.65)) ;
#18647 = CARTESIAN_POINT('',(68.6,49.65,11.65)) ;
#18648 = CARTESIAN_POINT('Origin',(78.25,49.65,11.65)) ;
#18649 = CARTESIAN_POINT('',(67.9,49.95,11.65)) ;
#18650 = CARTESIAN_POINT('Origin',(84.25,49.65,11.65)) ;
#18651 = CARTESIAN_POINT('',(72.25,49.65,11.65)) ;
#18652 = CARTESIAN_POINT('Origin',(78.25,49.65,11.65)) ;
#18653 = CARTESIAN_POINT('Origin',(78.25,49.15,11.65)) ;
#18654 = CARTESIAN_POINT('',(72.25,48.65,11.65)) ;
#18655 = CARTESIAN_POINT('Origin',(78.25,48.65,11.65)) ;
#18656 = CARTESIAN_POINT('',(72.25,49.15,11.65)) ;
#18657 = CARTESIAN_POINT('Origin',(80.3,48.65,11.65)) ;
#18658 = CARTESIAN_POINT('',(76.2,48.65,11.65)) ;
#18659 = CARTESIAN_POINT('Origin',(78.25,48.65,11.65)) ;
#18660 = CARTESIAN_POINT('Origin',(78.25,52.3,11.65)) ;
#18661 = CARTESIAN_POINT('',(76.2,52.3,11.65)) ;
#18662 = CARTESIAN_POINT('',(0.,0.,0.)) ;
#18663 = CARTESIAN_POINT('',(0.,0.,116.3)) ;
#18664 = CARTESIAN_POINT('',(2.99153807433531,0.,75.5811801535402)) ;
#18665 = CARTESIAN_POINT('',(69.1124627729124,0.,76.1599377291323)) ;
#18666 = CARTESIAN_POINT('',(0.,0.,0.)) ;
#18667 = CARTESIAN_POINT('',(0.,0.,0.)) ;
#18668 = CARTESIAN_POINT('',(72.414217553314,0.,116.3)) ;
#18669 = CARTESIAN_POINT('',(11.4409375366559,0.,88.4416441450611)) ;
#18670 = CARTESIAN_POINT('',(0.381381672463921,0.,118.878729070254)) ;
#18671 = CARTESIAN_POINT('',(0.,0.,0.)) ;
#18672 = CARTESIAN_POINT('',(0.,0.,0.)) ;
#18673 = CARTESIAN_POINT('',(0.,0.,0.)) ;
#18674 = CARTESIAN_POINT('',(0.,0.,0.)) ;
#18675 = CARTESIAN_POINT('',(0.,0.,0.)) ;
#18676 = CARTESIAN_POINT('',(0.,0.,0.)) ;
#18677 = CARTESIAN_POINT('',(0.,0.,0.)) ;
#18678 = CARTESIAN_POINT('',(0.,0.,0.)) ;
#18679 = CARTESIAN_POINT('',(0.,0.,70.)) ;
#18680 = CARTESIAN_POINT('',(0.,0.,70.)) ;
#18681 = CARTESIAN_POINT('',(-36.1403859968319,-7.5,62.85)) ;
#18682 = CARTESIAN_POINT('',(-36.1403859968319,-7.5,62.85)) ;
#18683 = CARTESIAN_POINT('',(-36.1403859968319,7.5,132.85)) ;
#18684 = CARTESIAN_POINT('',(-36.1403859968319,7.5,132.85)) ;
#18685 = CARTESIAN_POINT('',(0.,-5.09999999999999,125.7)) ;
#18686 = CARTESIAN_POINT('',(0.,-5.09999999999999,125.7)) ;
#18687 = CARTESIAN_POINT('',(0.,5.09999999999999,195.7)) ;
#18688 = CARTESIAN_POINT('',(0.,5.09999999999999,195.7)) ;
#18689 = CARTESIAN_POINT('',(5.,-52.,0.)) ;
#18690 = CARTESIAN_POINT('',(5.,-52.,0.)) ;
#18691 = CARTESIAN_POINT('',(18.25,-7.19999999999999,125.)) ;
#18692 = CARTESIAN_POINT('',(18.25,-7.19999999999999,125.)) ;
#18693 = CARTESIAN_POINT('',(24.,-48.2,17.)) ;
#18694 = CARTESIAN_POINT('',(24.,-48.2,17.)) ;
#18695 = CARTESIAN_POINT('',(6.25,2.15,-23.35)) ;
#18696 = CARTESIAN_POINT('',(6.25,2.15,-23.35)) ;
#18697 = CARTESIAN_POINT('',(6.25,-2.15,46.65)) ;
#18698 = CARTESIAN_POINT('',(6.25,-2.15,46.65)) ;
#18699 = CARTESIAN_POINT('',(-150.25,2.15,-23.35)) ;
#18700 = CARTESIAN_POINT('',(-150.25,2.15,-23.35)) ;
#18701 = CARTESIAN_POINT('',(-150.25,-2.15,46.65)) ;
#18702 = CARTESIAN_POINT('',(-150.25,-2.15,46.65)) ;
#18703 = CARTESIAN_POINT('',(72.414217553314,0.,205.1)) ;
#18704 = CARTESIAN_POINT('',(72.414217553314,89.1,79.4)) ;
#18705 = CARTESIAN_POINT('',(72.414217553314,-89.1,-9.4)) ;
#18706 = CARTESIAN_POINT('',(-13.,0.,0.)) ;
#18707 = CARTESIAN_POINT('',(0.,-104.6,0.)) ;
#18708 = CARTESIAN_POINT('',(-13.,-104.6,0.)) ;
#18709 = CARTESIAN_POINT('',(-156.5,0.,0.)) ;
#18710 = CARTESIAN_POINT('',(-169.5,0.,0.)) ;
#18711 = CARTESIAN_POINT('',(-156.5,-104.6,0.)) ;
#18712 = CARTESIAN_POINT('',(-169.5,-104.6,0.)) ;
#18713 = CARTESIAN_POINT('',(114.65,-7.3,-34.75)) ;
#18714 = CARTESIAN_POINT('',(114.65,-97.3,-34.75)) ;
#18715 = CARTESIAN_POINT('',(156.5,-9.58286120332804E-15,0.)) ;
#18716 = CARTESIAN_POINT('',(-156.5,9.58286120332804E-15,0.)) ;
#18717 = CARTESIAN_POINT('',(156.5,-9.58286120332804E-15,0.)) ;
#18718 = CARTESIAN_POINT('',(-156.5,0.,0.)) ;
#18719 = CARTESIAN_POINT('',(0.,-9.58286120332804E-16,0.)) ;
#18720 = UNCERTAINTY_MEASURE_WITH_UNIT(LENGTH_MEASURE(0.01),#18758,
'DISTANCE_ACCURACY_VALUE',
'Maximum model space distance between geometric entities at asserted c
onnectivities') ;
#18721 = UNCERTAINTY_MEASURE_WITH_UNIT(LENGTH_MEASURE(0.01),#18758,
'DISTANCE_ACCURACY_VALUE',
'Maximum model space distance between geometric entities at asserted c
onnectivities') ;
#18722 = UNCERTAINTY_MEASURE_WITH_UNIT(LENGTH_MEASURE(0.01),#18758,
'DISTANCE_ACCURACY_VALUE',
'Maximum model space distance between geometric entities at asserted c
onnectivities') ;
#18723 = UNCERTAINTY_MEASURE_WITH_UNIT(LENGTH_MEASURE(0.01),#18758,
'DISTANCE_ACCURACY_VALUE',
'Maximum model space distance between geometric entities at asserted c
onnectivities') ;
#18724 = UNCERTAINTY_MEASURE_WITH_UNIT(LENGTH_MEASURE(0.01),#18758,
'DISTANCE_ACCURACY_VALUE',
'Maximum model space distance between geometric entities at asserted c
onnectivities') ;
#18725 = UNCERTAINTY_MEASURE_WITH_UNIT(LENGTH_MEASURE(0.01),#18758,
'DISTANCE_ACCURACY_VALUE',
'Maximum model space distance between geometric entities at asserted c
onnectivities') ;
#18726 = UNCERTAINTY_MEASURE_WITH_UNIT(LENGTH_MEASURE(0.01),#18758,
'DISTANCE_ACCURACY_VALUE',
'Maximum model space distance between geometric entities at asserted c
onnectivities') ;
#18727 = UNCERTAINTY_MEASURE_WITH_UNIT(LENGTH_MEASURE(0.01),#18758,
'DISTANCE_ACCURACY_VALUE',
'Maximum model space distance between geometric entities at asserted c
onnectivities') ;
#18728 = UNCERTAINTY_MEASURE_WITH_UNIT(LENGTH_MEASURE(0.01),#18758,
'DISTANCE_ACCURACY_VALUE',
'Maximum model space distance between geometric entities at asserted c
onnectivities') ;
#18729 = UNCERTAINTY_MEASURE_WITH_UNIT(LENGTH_MEASURE(0.01),#18758,
'DISTANCE_ACCURACY_VALUE',
'Maximum model space distance between geometric entities at asserted c
onnectivities') ;
#18730 = UNCERTAINTY_MEASURE_WITH_UNIT(LENGTH_MEASURE(0.01),#18758,
'DISTANCE_ACCURACY_VALUE',
'Maximum model space distance between geometric entities at asserted c
onnectivities') ;
#18731 = UNCERTAINTY_MEASURE_WITH_UNIT(LENGTH_MEASURE(0.01),#18758,
'DISTANCE_ACCURACY_VALUE',
'Maximum model space distance between geometric entities at asserted c
onnectivities') ;
#18732 = UNCERTAINTY_MEASURE_WITH_UNIT(LENGTH_MEASURE(0.01),#18758,
'DISTANCE_ACCURACY_VALUE',
'Maximum model space distance between geometric entities at asserted c
onnectivities') ;
#18733 = UNCERTAINTY_MEASURE_WITH_UNIT(LENGTH_MEASURE(0.01),#18758,
'DISTANCE_ACCURACY_VALUE',
'Maximum model space distance between geometric entities at asserted c
onnectivities') ;
#18734 = UNCERTAINTY_MEASURE_WITH_UNIT(LENGTH_MEASURE(0.01),#18758,
'DISTANCE_ACCURACY_VALUE',
'Maximum model space distance between geometric entities at asserted c
onnectivities') ;
#18735 = UNCERTAINTY_MEASURE_WITH_UNIT(LENGTH_MEASURE(0.01),#18758,
'DISTANCE_ACCURACY_VALUE',
'Maximum model space distance between geometric entities at asserted c
onnectivities') ;
#18736 = UNCERTAINTY_MEASURE_WITH_UNIT(LENGTH_MEASURE(0.01),#18758,
'DISTANCE_ACCURACY_VALUE',
'Maximum model space distance between geometric entities at asserted c
onnectivities') ;
#18737 = UNCERTAINTY_MEASURE_WITH_UNIT(LENGTH_MEASURE(0.01),#18758,
'DISTANCE_ACCURACY_VALUE',
'Maximum model space distance between geometric entities at asserted c
onnectivities') ;
#18738 = UNCERTAINTY_MEASURE_WITH_UNIT(LENGTH_MEASURE(0.01),#18758,
'DISTANCE_ACCURACY_VALUE',
'Maximum model space distance between geometric entities at asserted c
onnectivities') ;
#18739 = (
GEOMETRIC_REPRESENTATION_CONTEXT(3)
GLOBAL_UNCERTAINTY_ASSIGNED_CONTEXT((#18720))
GLOBAL_UNIT_ASSIGNED_CONTEXT((#18758,#18760,#18761))
REPRESENTATION_CONTEXT('','3D')
) ;
#18740 = (
GEOMETRIC_REPRESENTATION_CONTEXT(3)
GLOBAL_UNCERTAINTY_ASSIGNED_CONTEXT((#18721))
GLOBAL_UNIT_ASSIGNED_CONTEXT((#18758,#18760,#18761))
REPRESENTATION_CONTEXT('','3D')
) ;
#18741 = (
GEOMETRIC_REPRESENTATION_CONTEXT(3)
GLOBAL_UNCERTAINTY_ASSIGNED_CONTEXT((#18722))
GLOBAL_UNIT_ASSIGNED_CONTEXT((#18758,#18760,#18761))
REPRESENTATION_CONTEXT('','3D')
) ;
#18742 = (
GEOMETRIC_REPRESENTATION_CONTEXT(3)
GLOBAL_UNCERTAINTY_ASSIGNED_CONTEXT((#18723))
GLOBAL_UNIT_ASSIGNED_CONTEXT((#18758,#18760,#18761))
REPRESENTATION_CONTEXT('','3D')
) ;
#18743 = (
GEOMETRIC_REPRESENTATION_CONTEXT(3)
GLOBAL_UNCERTAINTY_ASSIGNED_CONTEXT((#18724))
GLOBAL_UNIT_ASSIGNED_CONTEXT((#18758,#18760,#18761))
REPRESENTATION_CONTEXT('','3D')
) ;
#18744 = (
GEOMETRIC_REPRESENTATION_CONTEXT(3)
GLOBAL_UNCERTAINTY_ASSIGNED_CONTEXT((#18725))
GLOBAL_UNIT_ASSIGNED_CONTEXT((#18758,#18760,#18761))
REPRESENTATION_CONTEXT('','3D')
) ;
#18745 = (
GEOMETRIC_REPRESENTATION_CONTEXT(3)
GLOBAL_UNCERTAINTY_ASSIGNED_CONTEXT((#18726))
GLOBAL_UNIT_ASSIGNED_CONTEXT((#18758,#18760,#18761))
REPRESENTATION_CONTEXT('','3D')
) ;
#18746 = (
GEOMETRIC_REPRESENTATION_CONTEXT(3)
GLOBAL_UNCERTAINTY_ASSIGNED_CONTEXT((#18727))
GLOBAL_UNIT_ASSIGNED_CONTEXT((#18758,#18760,#18761))
REPRESENTATION_CONTEXT('','3D')
) ;
#18747 = (
GEOMETRIC_REPRESENTATION_CONTEXT(3)
GLOBAL_UNCERTAINTY_ASSIGNED_CONTEXT((#18728))
GLOBAL_UNIT_ASSIGNED_CONTEXT((#18758,#18760,#18761))
REPRESENTATION_CONTEXT('','3D')
) ;
#18748 = (
GEOMETRIC_REPRESENTATION_CONTEXT(3)
GLOBAL_UNCERTAINTY_ASSIGNED_CONTEXT((#18729))
GLOBAL_UNIT_ASSIGNED_CONTEXT((#18758,#18760,#18761))
REPRESENTATION_CONTEXT('','3D')
) ;
#18749 = (
GEOMETRIC_REPRESENTATION_CONTEXT(3)
GLOBAL_UNCERTAINTY_ASSIGNED_CONTEXT((#18730))
GLOBAL_UNIT_ASSIGNED_CONTEXT((#18758,#18760,#18761))
REPRESENTATION_CONTEXT('','3D')
) ;
#18750 = (
GEOMETRIC_REPRESENTATION_CONTEXT(3)
GLOBAL_UNCERTAINTY_ASSIGNED_CONTEXT((#18731))
GLOBAL_UNIT_ASSIGNED_CONTEXT((#18758,#18760,#18761))
REPRESENTATION_CONTEXT('','3D')
) ;
#18751 = (
GEOMETRIC_REPRESENTATION_CONTEXT(3)
GLOBAL_UNCERTAINTY_ASSIGNED_CONTEXT((#18732))
GLOBAL_UNIT_ASSIGNED_CONTEXT((#18758,#18760,#18761))
REPRESENTATION_CONTEXT('','3D')
) ;
#18752 = (
GEOMETRIC_REPRESENTATION_CONTEXT(3)
GLOBAL_UNCERTAINTY_ASSIGNED_CONTEXT((#18733))
GLOBAL_UNIT_ASSIGNED_CONTEXT((#18758,#18760,#18761))
REPRESENTATION_CONTEXT('','3D')
) ;
#18753 = (
GEOMETRIC_REPRESENTATION_CONTEXT(3)
GLOBAL_UNCERTAINTY_ASSIGNED_CONTEXT((#18734))
GLOBAL_UNIT_ASSIGNED_CONTEXT((#18758,#18760,#18761))
REPRESENTATION_CONTEXT('','3D')
) ;
#18754 = (
GEOMETRIC_REPRESENTATION_CONTEXT(3)
GLOBAL_UNCERTAINTY_ASSIGNED_CONTEXT((#18735))
GLOBAL_UNIT_ASSIGNED_CONTEXT((#18758,#18760,#18761))
REPRESENTATION_CONTEXT('','3D')
) ;
#18755 = (
GEOMETRIC_REPRESENTATION_CONTEXT(3)
GLOBAL_UNCERTAINTY_ASSIGNED_CONTEXT((#18736))
GLOBAL_UNIT_ASSIGNED_CONTEXT((#18758,#18760,#18761))
REPRESENTATION_CONTEXT('','3D')
) ;
#18756 = (
GEOMETRIC_REPRESENTATION_CONTEXT(3)
GLOBAL_UNCERTAINTY_ASSIGNED_CONTEXT((#18737))
GLOBAL_UNIT_ASSIGNED_CONTEXT((#18758,#18760,#18761))
REPRESENTATION_CONTEXT('','3D')
) ;
#18757 = (
GEOMETRIC_REPRESENTATION_CONTEXT(3)
GLOBAL_UNCERTAINTY_ASSIGNED_CONTEXT((#18738))
GLOBAL_UNIT_ASSIGNED_CONTEXT((#18758,#18760,#18761))
REPRESENTATION_CONTEXT('','3D')
) ;
#18758 = (
LENGTH_UNIT()
NAMED_UNIT(*)
SI_UNIT(.MILLI.,.METRE.)
) ;
#18759 = (
LENGTH_UNIT()
NAMED_UNIT(*)
SI_UNIT($,.METRE.)
) ;
#18760 = (
NAMED_UNIT(*)
PLANE_ANGLE_UNIT()
SI_UNIT($,.RADIAN.)
) ;
#18761 = (
NAMED_UNIT(*)
SI_UNIT($,.STERADIAN.)
SOLID_ANGLE_UNIT()
) ;
#18762 = SHAPE_DEFINITION_REPRESENTATION(#18780,#18856) ;
#18763 = SHAPE_DEFINITION_REPRESENTATION(#18781,#18857) ;
#18764 = SHAPE_DEFINITION_REPRESENTATION(#18782,#18858) ;
#18765 = SHAPE_DEFINITION_REPRESENTATION(#18783,#18859) ;
#18766 = SHAPE_DEFINITION_REPRESENTATION(#18784,#18860) ;
#18767 = SHAPE_DEFINITION_REPRESENTATION(#18785,#18861) ;
#18768 = SHAPE_DEFINITION_REPRESENTATION(#18786,#18862) ;
#18769 = SHAPE_DEFINITION_REPRESENTATION(#18787,#18863) ;
#18770 = SHAPE_DEFINITION_REPRESENTATION(#18788,#18864) ;
#18771 = SHAPE_DEFINITION_REPRESENTATION(#18789,#18865) ;
#18772 = SHAPE_DEFINITION_REPRESENTATION(#18790,#18866) ;
#18773 = SHAPE_DEFINITION_REPRESENTATION(#18791,#18867) ;
#18774 = SHAPE_DEFINITION_REPRESENTATION(#18792,#18868) ;
#18775 = SHAPE_DEFINITION_REPRESENTATION(#18793,#18869) ;
#18776 = SHAPE_DEFINITION_REPRESENTATION(#18794,#18870) ;
#18777 = SHAPE_DEFINITION_REPRESENTATION(#18795,#18871) ;
#18778 = SHAPE_DEFINITION_REPRESENTATION(#18796,#18872) ;
#18779 = SHAPE_DEFINITION_REPRESENTATION(#18797,#18873) ;
#18780 = PRODUCT_DEFINITION_SHAPE('',$,#18875) ;
#18781 = PRODUCT_DEFINITION_SHAPE('',$,#18876) ;
#18782 = PRODUCT_DEFINITION_SHAPE('',$,#18877) ;
#18783 = PRODUCT_DEFINITION_SHAPE('',$,#18878) ;
#18784 = PRODUCT_DEFINITION_SHAPE('',$,#18879) ;
#18785 = PRODUCT_DEFINITION_SHAPE('',$,#18880) ;
#18786 = PRODUCT_DEFINITION_SHAPE('',$,#18881) ;
#18787 = PRODUCT_DEFINITION_SHAPE('',$,#18882) ;
#18788 = PRODUCT_DEFINITION_SHAPE('',$,#18883) ;
#18789 = PRODUCT_DEFINITION_SHAPE('',$,#18884) ;
#18790 = PRODUCT_DEFINITION_SHAPE('',$,#18885) ;
#18791 = PRODUCT_DEFINITION_SHAPE('',$,#18886) ;
#18792 = PRODUCT_DEFINITION_SHAPE('',$,#18887) ;
#18793 = PRODUCT_DEFINITION_SHAPE('',$,#18888) ;
#18794 = PRODUCT_DEFINITION_SHAPE('',$,#18889) ;
#18795 = PRODUCT_DEFINITION_SHAPE('',$,#18890) ;
#18796 = PRODUCT_DEFINITION_SHAPE('',$,#18891) ;
#18797 = PRODUCT_DEFINITION_SHAPE('',$,#18892) ;
#18798 = PRODUCT_DEFINITION_SHAPE($,$,#185) ;
#18799 = PRODUCT_DEFINITION_SHAPE($,$,#186) ;
#18800 = PRODUCT_DEFINITION_SHAPE($,$,#187) ;
#18801 = PRODUCT_DEFINITION_SHAPE($,$,#188) ;
#18802 = PRODUCT_DEFINITION_SHAPE($,$,#189) ;
#18803 = PRODUCT_DEFINITION_SHAPE($,$,#190) ;
#18804 = PRODUCT_DEFINITION_SHAPE($,$,#191) ;
#18805 = PRODUCT_DEFINITION_SHAPE($,$,#192) ;
#18806 = PRODUCT_DEFINITION_SHAPE($,$,#193) ;
#18807 = PRODUCT_DEFINITION_SHAPE($,$,#194) ;
#18808 = PRODUCT_DEFINITION_SHAPE($,$,#195) ;
#18809 = PRODUCT_DEFINITION_SHAPE($,$,#196) ;
#18810 = PRODUCT_DEFINITION_SHAPE($,$,#197) ;
#18811 = PRODUCT_DEFINITION_SHAPE($,$,#198) ;
#18812 = PRODUCT_DEFINITION_SHAPE($,$,#199) ;
#18813 = PRODUCT_DEFINITION_SHAPE($,$,#200) ;
#18814 = PRODUCT_DEFINITION_SHAPE($,$,#201) ;
#18815 = PRODUCT_DEFINITION_SHAPE($,$,#202) ;
#18816 = PRODUCT_DEFINITION_SHAPE($,$,#203) ;
#18817 = PRODUCT_DEFINITION_SHAPE($,$,#204) ;
#18818 = PRODUCT_DEFINITION_SHAPE($,$,#205) ;
#18819 = PRODUCT_DEFINITION_SHAPE($,$,#206) ;
#18820 = PRODUCT_DEFINITION_SHAPE($,$,#207) ;
#18821 = PRODUCT_DEFINITION_SHAPE($,$,#208) ;
#18822 = PRODUCT_DEFINITION_SHAPE($,$,#209) ;
#18823 = PRODUCT_DEFINITION_SHAPE($,$,#210) ;
#18824 = PRODUCT_DEFINITION_SHAPE($,$,#211) ;
#18825 = PRODUCT_DEFINITION_SHAPE($,$,#212) ;
#18826 = PRODUCT_DEFINITION_SHAPE($,$,#213) ;
#18827 = PRODUCT_DEFINITION_SHAPE($,$,#214) ;
#18828 = PRODUCT_DEFINITION_SHAPE($,$,#215) ;
#18829 = PRODUCT_DEFINITION_SHAPE($,$,#216) ;
#18830 = PRODUCT_DEFINITION_SHAPE($,$,#217) ;
#18831 = PRODUCT_DEFINITION_SHAPE($,$,#218) ;
#18832 = PRODUCT_DEFINITION_SHAPE($,$,#219) ;
#18833 = PRODUCT_DEFINITION_SHAPE($,$,#220) ;
#18834 = PRODUCT_DEFINITION_SHAPE($,$,#221) ;
#18835 = PRODUCT_DEFINITION_SHAPE($,$,#222) ;
#18836 = PRODUCT_DEFINITION_SHAPE($,$,#223) ;
#18837 = PRODUCT_DEFINITION_SHAPE($,$,#224) ;
#18838 = PRODUCT_DEFINITION_SHAPE($,$,#225) ;
#18839 = PRODUCT_DEFINITION_SHAPE($,$,#226) ;
#18840 = PRODUCT_DEFINITION_SHAPE($,$,#227) ;
#18841 = PRODUCT_DEFINITION_SHAPE($,$,#228) ;
#18842 = PRODUCT_DEFINITION_SHAPE($,$,#229) ;
#18843 = PRODUCT_DEFINITION_SHAPE($,$,#230) ;
#18844 = PRODUCT_DEFINITION_SHAPE($,$,#231) ;
#18845 = PRODUCT_DEFINITION_SHAPE($,$,#232) ;
#18846 = PRODUCT_DEFINITION_SHAPE($,$,#233) ;
#18847 = PRODUCT_DEFINITION_SHAPE($,$,#234) ;
#18848 = PRODUCT_DEFINITION_SHAPE($,$,#235) ;
#18849 = PRODUCT_DEFINITION_SHAPE($,$,#236) ;
#18850 = PRODUCT_DEFINITION_SHAPE($,$,#237) ;
#18851 = PRODUCT_DEFINITION_SHAPE($,$,#238) ;
#18852 = PRODUCT_DEFINITION_SHAPE($,$,#239) ;
#18853 = PRODUCT_DEFINITION_SHAPE($,$,#240) ;
#18854 = PRODUCT_DEFINITION_SHAPE($,$,#241) ;
#18855 = PRODUCT_DEFINITION_SHAPE($,$,#242) ;
#18856 = SHAPE_REPRESENTATION('',(#9747,#10657,#10658,#10659,#10660,#10661,
#10662,#10663,#10664,#10665,#10666,#10667,#10668,#10669,#10670,#10671,#10672,
#10673,#10674,#10675,#10676,#10677,#10678,#10679,#10680,#10681,#10682,#10683,
#10684,#10685,#10686,#10687,#10688,#10689,#10690,#10691,#10692,#10693,#10694,
#10695,#10696,#10697,#10698,#10699,#10700,#10701,#10702,#10703,#10704,#10705,
#10706,#10707,#10708,#10709,#10710,#10711,#10712,#10713,#10714),#18739) ;
#18857 = SHAPE_REPRESENTATION('',(#9748),#18740) ;
#18858 = SHAPE_REPRESENTATION('',(#9905),#18741) ;
#18859 = SHAPE_REPRESENTATION('',(#9983),#18742) ;
#18860 = SHAPE_REPRESENTATION('',(#10025),#18743) ;
#18861 = SHAPE_REPRESENTATION('',(#10070),#18744) ;
#18862 = SHAPE_REPRESENTATION('',(#10098),#18745) ;
#18863 = SHAPE_REPRESENTATION('',(#10122),#18746) ;
#18864 = SHAPE_REPRESENTATION('',(#10152),#18747) ;
#18865 = SHAPE_REPRESENTATION('',(#10171),#18748) ;
#18866 = SHAPE_REPRESENTATION('',(#10205),#18749) ;
#18867 = SHAPE_REPRESENTATION('',(#10219),#18750) ;
#18868 = SHAPE_REPRESENTATION('',(#10241),#18751) ;
#18869 = SHAPE_REPRESENTATION('',(#10254),#18752) ;
#18870 = SHAPE_REPRESENTATION('',(#10270),#18753) ;
#18871 = SHAPE_REPRESENTATION('',(#10552),#18754) ;
#18872 = SHAPE_REPRESENTATION('',(#10599),#18755) ;
#18873 = SHAPE_REPRESENTATION('',(#10632),#18756) ;
#18874 = PRODUCT_DEFINITION_CONTEXT('part definition',#18930,'design') ;
#18875 = PRODUCT_DEFINITION('MAS-601','MAS-601',#18893,
#18874) ;
#18876 = PRODUCT_DEFINITION('Lift Table Base Frame Weldment',
'Lift Table Base Frame Weldment',#18894,#18874) ;
#18877 = PRODUCT_DEFINITION('Lift Table Top 14 ga with Pivot Lugs',
'Lift Table Top 14 ga with Pivot Lugs',#18895,#18874) ;
#18878 = PRODUCT_DEFINITION('Outer Scissor Arm Frame',
'Outer Scissor Arm Frame',#18896,#18874) ;
#18879 = PRODUCT_DEFINITION('Inner Scissor Arm Frame',
'Inner Scissor Arm Frame',#18897,#18874) ;
#18880 = PRODUCT_DEFINITION('Hydraulic Cylinder Body',
'Hydraulic Cylinder Body',#18898,#18874) ;
#18881 = PRODUCT_DEFINITION('Hydraulic Piston Rod with Eye',
'Hydraulic Piston Rod with Eye',#18899,#18874) ;
#18882 = PRODUCT_DEFINITION('Hydraulic Foot Pump Body',
'Hydraulic Foot Pump Body',#18900,#18874) ;
#18883 = PRODUCT_DEFINITION('Foot Pump Pedal','Foot Pump Pedal',#18901,
#18874) ;
#18884 = PRODUCT_DEFINITION('Push Handle (chrome tube)',
'Push Handle (chrome tube)',#18902,#18874) ;
#18885 = PRODUCT_DEFINITION('Lowering Release Lever',
'Lowering Release Lever',#18903,#18874) ;
#18886 = PRODUCT_DEFINITION('Pivot Pin D4 x 11.4 with E-Clip Groove',
'Pivot Pin D4 x 11.4 with E-Clip Groove',#18904,#18874) ;
#18887 = PRODUCT_DEFINITION('DIN 6799 - 3.2 Retaining Washer (E-Clip)',
'DIN 6799 - 3.2 Retaining Washer (E-Clip)',#18905,#18874) ;
#18888 = PRODUCT_DEFINITION('Track Roller D8 with Stud',
'Track Roller D8 with Stud',#18906,#18874) ;
#18889 = PRODUCT_DEFINITION('ISO 4762 - M2 x 6 - 12.9',
'ISO 4762 - M2 x 6 - 12.9',#18907,#18874) ;
#18890 = PRODUCT_DEFINITION('Swivel Caster Yoke 4 in',
'Swivel Caster Yoke 4 in',#18908,#18874) ;
#18891 = PRODUCT_DEFINITION('Rigid Caster Yoke 4 in',
'Rigid Caster Yoke 4 in',#18909,#18874) ;
#18892 = PRODUCT_DEFINITION('Caster Wheel 4 in Rubber',
'Caster Wheel 4 in Rubber',#18910,#18874) ;
#18893 = PRODUCT_DEFINITION_FORMATION('',$,#18932) ;
#18894 = PRODUCT_DEFINITION_FORMATION('',$,#18933) ;
#18895 = PRODUCT_DEFINITION_FORMATION('',$,#18934) ;
#18896 = PRODUCT_DEFINITION_FORMATION('',$,#18935) ;
#18897 = PRODUCT_DEFINITION_FORMATION('',$,#18936) ;
#18898 = PRODUCT_DEFINITION_FORMATION('',$,#18937) ;
#18899 = PRODUCT_DEFINITION_FORMATION('',$,#18938) ;
#18900 = PRODUCT_DEFINITION_FORMATION('',$,#18939) ;
#18901 = PRODUCT_DEFINITION_FORMATION('',$,#18940) ;
#18902 = PRODUCT_DEFINITION_FORMATION('',$,#18941) ;
#18903 = PRODUCT_DEFINITION_FORMATION('',$,#18942) ;
#18904 = PRODUCT_DEFINITION_FORMATION('',$,#18943) ;
#18905 = PRODUCT_DEFINITION_FORMATION('',$,#18944) ;
#18906 = PRODUCT_DEFINITION_FORMATION('',$,#18945) ;
#18907 = PRODUCT_DEFINITION_FORMATION('',$,#18946) ;
#18908 = PRODUCT_DEFINITION_FORMATION('',$,#18947) ;
#18909 = PRODUCT_DEFINITION_FORMATION('',$,#18948) ;
#18910 = PRODUCT_DEFINITION_FORMATION('',$,#18949) ;
#18911 = PRODUCT_RELATED_PRODUCT_CATEGORY('MAS-601','MAS-601',(#18932)) ;
#18912 = PRODUCT_RELATED_PRODUCT_CATEGORY(
'Lift Table Base Frame Weldment','Lift Table Base Frame Weldment',(#18933)) ;
#18913 = PRODUCT_RELATED_PRODUCT_CATEGORY(
'Lift Table Top 14 ga with Pivot Lugs',
'Lift Table Top 14 ga with Pivot Lugs',(#18934)) ;
#18914 = PRODUCT_RELATED_PRODUCT_CATEGORY('Outer Scissor Arm Frame',
'Outer Scissor Arm Frame',(#18935)) ;
#18915 = PRODUCT_RELATED_PRODUCT_CATEGORY('Inner Scissor Arm Frame',
'Inner Scissor Arm Frame',(#18936)) ;
#18916 = PRODUCT_RELATED_PRODUCT_CATEGORY('Hydraulic Cylinder Body',
'Hydraulic Cylinder Body',(#18937)) ;
#18917 = PRODUCT_RELATED_PRODUCT_CATEGORY('Hydraulic Piston Rod with Eye',
'Hydraulic Piston Rod with Eye',(#18938)) ;
#18918 = PRODUCT_RELATED_PRODUCT_CATEGORY('Hydraulic Foot Pump Body',
'Hydraulic Foot Pump Body',(#18939)) ;
#18919 = PRODUCT_RELATED_PRODUCT_CATEGORY('Foot Pump Pedal',
'Foot Pump Pedal',(#18940)) ;
#18920 = PRODUCT_RELATED_PRODUCT_CATEGORY('Push Handle (chrome tube)',
'Push Handle (chrome tube)',(#18941)) ;
#18921 = PRODUCT_RELATED_PRODUCT_CATEGORY('Lowering Release Lever',
'Lowering Release Lever',(#18942)) ;
#18922 = PRODUCT_RELATED_PRODUCT_CATEGORY(
'Pivot Pin D4 x 11.4 with E-Clip Groove',
'Pivot Pin D4 x 11.4 with E-Clip Groove',(#18943)) ;
#18923 = PRODUCT_RELATED_PRODUCT_CATEGORY(
'DIN 6799 - 3.2 Retaining Washer (E-Clip)',
'DIN 6799 - 3.2 Retaining Washer (E-Clip)',(#18944)) ;
#18924 = PRODUCT_RELATED_PRODUCT_CATEGORY('Track Roller D8 with Stud',
'Track Roller D8 with Stud',(#18945)) ;
#18925 = PRODUCT_RELATED_PRODUCT_CATEGORY('ISO 4762 - M2 x 6 - 12.9',
'ISO 4762 - M2 x 6 - 12.9',(#18946)) ;
#18926 = PRODUCT_RELATED_PRODUCT_CATEGORY('Swivel Caster Yoke 4 in',
'Swivel Caster Yoke 4 in',(#18947)) ;
#18927 = PRODUCT_RELATED_PRODUCT_CATEGORY('Rigid Caster Yoke 4 in',
'Rigid Caster Yoke 4 in',(#18948)) ;
#18928 = PRODUCT_RELATED_PRODUCT_CATEGORY('Caster Wheel 4 in Rubber',
'Caster Wheel 4 in Rubber',(#18949)) ;
#18929 = APPLICATION_PROTOCOL_DEFINITION('international standard',
'automotive_design',2009,#18930) ;
#18930 = APPLICATION_CONTEXT(
'Core Data for Automotive Mechanical Design Process') ;
#18931 = PRODUCT_CONTEXT('part definition',#18930,'mechanical') ;
#18932 = PRODUCT('MAS-601','MAS-601',$,(#18931)) ;
#18933 = PRODUCT('Lift Table Base Frame Weldment',
'Lift Table Base Frame Weldment',$,(#18931)) ;
#18934 = PRODUCT('Lift Table Top 14 ga with Pivot Lugs',
'Lift Table Top 14 ga with Pivot Lugs',$,(#18931)) ;
#18935 = PRODUCT('Outer Scissor Arm Frame','Outer Scissor Arm Frame',$,(#18931)) ;
#18936 = PRODUCT('Inner Scissor Arm Frame','Inner Scissor Arm Frame',$,(#18931)) ;
#18937 = PRODUCT('Hydraulic Cylinder Body','Hydraulic Cylinder Body',$,(#18931)) ;
#18938 = PRODUCT('Hydraulic Piston Rod with Eye',
'Hydraulic Piston Rod with Eye',$,(#18931)) ;
#18939 = PRODUCT('Hydraulic Foot Pump Body','Hydraulic Foot Pump Body',$,(#18931)) ;
#18940 = PRODUCT('Foot Pump Pedal','Foot Pump Pedal',$,(#18931)) ;
#18941 = PRODUCT('Push Handle (chrome tube)','Push Handle (chrome tube)',$,
(#18931)) ;
#18942 = PRODUCT('Lowering Release Lever','Lowering Release Lever',$,(#18931)) ;
#18943 = PRODUCT('Pivot Pin D4 x 11.4 with E-Clip Groove',
'Pivot Pin D4 x 11.4 with E-Clip Groove',$,(#18931)) ;
#18944 = PRODUCT('DIN 6799 - 3.2 Retaining Washer (E-Clip)',
'DIN 6799 - 3.2 Retaining Washer (E-Clip)',$,(#18931)) ;
#18945 = PRODUCT('Track Roller D8 with Stud','Track Roller D8 with Stud',$,
(#18931)) ;
#18946 = PRODUCT('ISO 4762 - M2 x 6 - 12.9','ISO 4762 - M2 x 6 - 12.9',$,(#18931)) ;
#18947 = PRODUCT('Swivel Caster Yoke 4 in','Swivel Caster Yoke 4 in',$,(#18931)) ;
#18948 = PRODUCT('Rigid Caster Yoke 4 in','Rigid Caster Yoke 4 in',$,(#18931)) ;
#18949 = PRODUCT('Caster Wheel 4 in Rubber','Caster Wheel 4 in Rubber',$,(#18931)) ;
#18950 = PRESENTATION_STYLE_ASSIGNMENT((#18968)) ;
#18951 = PRESENTATION_STYLE_ASSIGNMENT((#18969)) ;
#18952 = PRESENTATION_STYLE_ASSIGNMENT((#18970)) ;
#18953 = PRESENTATION_STYLE_ASSIGNMENT((#18971)) ;
#18954 = PRESENTATION_STYLE_ASSIGNMENT((#18972)) ;
#18955 = PRESENTATION_STYLE_ASSIGNMENT((#18973)) ;
#18956 = PRESENTATION_STYLE_ASSIGNMENT((#18974)) ;
#18957 = PRESENTATION_STYLE_ASSIGNMENT((#18975)) ;
#18958 = PRESENTATION_STYLE_ASSIGNMENT((#18976)) ;
#18959 = PRESENTATION_STYLE_ASSIGNMENT((#18977)) ;
#18960 = PRESENTATION_STYLE_ASSIGNMENT((#18978)) ;
#18961 = PRESENTATION_STYLE_ASSIGNMENT((#18979)) ;
#18962 = PRESENTATION_STYLE_ASSIGNMENT((#18980)) ;
#18963 = PRESENTATION_STYLE_ASSIGNMENT((#18981)) ;
#18964 = PRESENTATION_STYLE_ASSIGNMENT((#18982)) ;
#18965 = PRESENTATION_STYLE_ASSIGNMENT((#18983)) ;
#18966 = PRESENTATION_STYLE_ASSIGNMENT((#18984)) ;
#18967 = PRESENTATION_STYLE_ASSIGNMENT((#18985)) ;
#18968 = SURFACE_STYLE_USAGE(.BOTH.,#18986) ;
#18969 = SURFACE_STYLE_USAGE(.BOTH.,#18987) ;
#18970 = SURFACE_STYLE_USAGE(.BOTH.,#18988) ;
#18971 = SURFACE_STYLE_USAGE(.BOTH.,#18989) ;
#18972 = SURFACE_STYLE_USAGE(.BOTH.,#18990) ;
#18973 = SURFACE_STYLE_USAGE(.BOTH.,#18991) ;
#18974 = SURFACE_STYLE_USAGE(.BOTH.,#18992) ;
#18975 = SURFACE_STYLE_USAGE(.BOTH.,#18993) ;
#18976 = SURFACE_STYLE_USAGE(.BOTH.,#18994) ;
#18977 = SURFACE_STYLE_USAGE(.BOTH.,#18995) ;
#18978 = SURFACE_STYLE_USAGE(.BOTH.,#18996) ;
#18979 = SURFACE_STYLE_USAGE(.BOTH.,#18997) ;
#18980 = SURFACE_STYLE_USAGE(.BOTH.,#18998) ;
#18981 = SURFACE_STYLE_USAGE(.BOTH.,#18999) ;
#18982 = SURFACE_STYLE_USAGE(.BOTH.,#19000) ;
#18983 = SURFACE_STYLE_USAGE(.BOTH.,#19001) ;
#18984 = SURFACE_STYLE_USAGE(.BOTH.,#19002) ;
#18985 = SURFACE_STYLE_USAGE(.BOTH.,#19003) ;
#18986 = SURFACE_SIDE_STYLE('',(#19004)) ;
#18987 = SURFACE_SIDE_STYLE('',(#19005)) ;
#18988 = SURFACE_SIDE_STYLE('',(#19006)) ;
#18989 = SURFACE_SIDE_STYLE('',(#19007)) ;
#18990 = SURFACE_SIDE_STYLE('',(#19008)) ;
#18991 = SURFACE_SIDE_STYLE('',(#19009)) ;
#18992 = SURFACE_SIDE_STYLE('',(#19010)) ;
#18993 = SURFACE_SIDE_STYLE('',(#19011)) ;
#18994 = SURFACE_SIDE_STYLE('',(#19012)) ;
#18995 = SURFACE_SIDE_STYLE('',(#19013)) ;
#18996 = SURFACE_SIDE_STYLE('',(#19014)) ;
#18997 = SURFACE_SIDE_STYLE('',(#19015)) ;
#18998 = SURFACE_SIDE_STYLE('',(#19016)) ;
#18999 = SURFACE_SIDE_STYLE('',(#19017)) ;
#19000 = SURFACE_SIDE_STYLE('',(#19018)) ;
#19001 = SURFACE_SIDE_STYLE('',(#19019)) ;
#19002 = SURFACE_SIDE_STYLE('',(#19020)) ;
#19003 = SURFACE_SIDE_STYLE('',(#19021)) ;
#19004 = SURFACE_STYLE_FILL_AREA(#19022) ;
#19005 = SURFACE_STYLE_FILL_AREA(#19023) ;
#19006 = SURFACE_STYLE_FILL_AREA(#19024) ;
#19007 = SURFACE_STYLE_FILL_AREA(#19025) ;
#19008 = SURFACE_STYLE_FILL_AREA(#19026) ;
#19009 = SURFACE_STYLE_FILL_AREA(#19027) ;
#19010 = SURFACE_STYLE_FILL_AREA(#19028) ;
#19011 = SURFACE_STYLE_FILL_AREA(#19029) ;
#19012 = SURFACE_STYLE_FILL_AREA(#19030) ;
#19013 = SURFACE_STYLE_FILL_AREA(#19031) ;
#19014 = SURFACE_STYLE_FILL_AREA(#19032) ;
#19015 = SURFACE_STYLE_FILL_AREA(#19033) ;
#19016 = SURFACE_STYLE_FILL_AREA(#19034) ;
#19017 = SURFACE_STYLE_FILL_AREA(#19035) ;
#19018 = SURFACE_STYLE_FILL_AREA(#19036) ;
#19019 = SURFACE_STYLE_FILL_AREA(#19037) ;
#19020 = SURFACE_STYLE_FILL_AREA(#19038) ;
#19021 = SURFACE_STYLE_FILL_AREA(#19039) ;
#19022 = FILL_AREA_STYLE('Steel - Satin',(#19040)) ;
#19023 = FILL_AREA_STYLE(
'MAS-253 Metallic Sheet - Lift Table Base Frame Weldment',(#19041)) ;
#19024 = FILL_AREA_STYLE(
'MAS-253 Metallic Sheet - Lift Table Top 14 ga with Pivot Lugs',(#19042)) ;
#19025 = FILL_AREA_STYLE(
'MAS-253 Metallic Sheet - Outer Scissor Arm Frame',(#19043)) ;
#19026 = FILL_AREA_STYLE(
'MAS-253 Metallic Sheet - Inner Scissor Arm Frame',(#19044)) ;
#19027 = FILL_AREA_STYLE(
'MAS-253 Metallic Sheet - Hydraulic Cylinder Body',(#19045)) ;
#19028 = FILL_AREA_STYLE(
'MAS-253 Metallic Sheet - Hydraulic Piston Rod with Eye',(#19046)) ;
#19029 = FILL_AREA_STYLE(
'MAS-253 Metallic Sheet - Hydraulic Foot Pump Body',(#19047)) ;
#19030 = FILL_AREA_STYLE('MAS-253 Metallic Sheet - Foot Pump Pedal',(#19048)) ;
#19031 = FILL_AREA_STYLE(
'MAS-253 Metallic Sheet - Push Handle (chrome tube)',(#19049)) ;
#19032 = FILL_AREA_STYLE(
'MAS-253 Metallic Sheet - Lowering Release Lever',(#19050)) ;
#19033 = FILL_AREA_STYLE(
'MAS-253 Metallic Sheet - Pivot Pin D4 x 11.4 with E-Clip Groove',(#19051)) ;
#19034 = FILL_AREA_STYLE(
'MAS-253 Metallic Sheet - DIN 6799 - 3.2 Retaining Washer (E-Clip)',(#19052)) ;
#19035 = FILL_AREA_STYLE(
'MAS-253 Metallic Sheet - Track Roller D8 with Stud',(#19053)) ;
#19036 = FILL_AREA_STYLE(
'MAS-253 Metallic Sheet - ISO 4762 - M2 x 6 - 12.9',(#19054)) ;
#19037 = FILL_AREA_STYLE(
'MAS-253 Metallic Sheet - Swivel Caster Yoke 4 in',(#19055)) ;
#19038 = FILL_AREA_STYLE(
'MAS-253 Metallic Sheet - Rigid Caster Yoke 4 in',(#19056)) ;
#19039 = FILL_AREA_STYLE(
'MAS-253 Metallic Sheet - Caster Wheel 4 in Rubber',(#19057)) ;
#19040 = FILL_AREA_STYLE_COLOUR('Steel - Satin',#19058) ;
#19041 = FILL_AREA_STYLE_COLOUR(
'MAS-253 Metallic Sheet - Lift Table Base Frame Weldment',#19059) ;
#19042 = FILL_AREA_STYLE_COLOUR(
'MAS-253 Metallic Sheet - Lift Table Top 14 ga with Pivot Lugs',#19060) ;
#19043 = FILL_AREA_STYLE_COLOUR(
'MAS-253 Metallic Sheet - Outer Scissor Arm Frame',#19061) ;
#19044 = FILL_AREA_STYLE_COLOUR(
'MAS-253 Metallic Sheet - Inner Scissor Arm Frame',#19062) ;
#19045 = FILL_AREA_STYLE_COLOUR(
'MAS-253 Metallic Sheet - Hydraulic Cylinder Body',#19063) ;
#19046 = FILL_AREA_STYLE_COLOUR(
'MAS-253 Metallic Sheet - Hydraulic Piston Rod with Eye',#19064) ;
#19047 = FILL_AREA_STYLE_COLOUR(
'MAS-253 Metallic Sheet - Hydraulic Foot Pump Body',#19065) ;
#19048 = FILL_AREA_STYLE_COLOUR(
'MAS-253 Metallic Sheet - Foot Pump Pedal',#19066) ;
#19049 = FILL_AREA_STYLE_COLOUR(
'MAS-253 Metallic Sheet - Push Handle (chrome tube)',#19067) ;
#19050 = FILL_AREA_STYLE_COLOUR(
'MAS-253 Metallic Sheet - Lowering Release Lever',#19068) ;
#19051 = FILL_AREA_STYLE_COLOUR(
'MAS-253 Metallic Sheet - Pivot Pin D4 x 11.4 with E-Clip Groove',#19069) ;
#19052 = FILL_AREA_STYLE_COLOUR(
'MAS-253 Metallic Sheet - DIN 6799 - 3.2 Retaining Washer (E-Clip)',#19070) ;
#19053 = FILL_AREA_STYLE_COLOUR(
'MAS-253 Metallic Sheet - Track Roller D8 with Stud',#19071) ;
#19054 = FILL_AREA_STYLE_COLOUR(
'MAS-253 Metallic Sheet - ISO 4762 - M2 x 6 - 12.9',#19072) ;
#19055 = FILL_AREA_STYLE_COLOUR(
'MAS-253 Metallic Sheet - Swivel Caster Yoke 4 in',#19073) ;
#19056 = FILL_AREA_STYLE_COLOUR(
'MAS-253 Metallic Sheet - Rigid Caster Yoke 4 in',#19074) ;
#19057 = FILL_AREA_STYLE_COLOUR(
'MAS-253 Metallic Sheet - Caster Wheel 4 in Rubber',#19075) ;
#19058 = COLOUR_RGB('Steel - Satin', 0.66274510, 0.83137255, 0.94901961) ;
#19059 = COLOUR_RGB(
'MAS-253 Metallic Sheet - Lift Table Base Frame Weldment', 0.66274510, 0.83137255, 0.94901961) ;
#19060 = COLOUR_RGB(
'MAS-253 Metallic Sheet - Lift Table Top 14 ga with Pivot Lugs', 0.31764706, 0.68627451, 0.89019608) ;
#19061 = COLOUR_RGB('MAS-253 Metallic Sheet - Outer Scissor Arm Frame', 0.40784314, 0.44705882, 0.49803922) ;
#19062 = COLOUR_RGB('MAS-253 Metallic Sheet - Inner Scissor Arm Frame', 0.72549020, 0.75294118, 0.79215686) ;
#19063 = COLOUR_RGB('MAS-253 Metallic Sheet - Hydraulic Cylinder Body', 0.08235294, 0.09019608, 0.10196078) ;
#19064 = COLOUR_RGB(
'MAS-253 Metallic Sheet - Hydraulic Piston Rod with Eye', 0.09019608, 0.27058824, 0.51372549) ;
#19065 = COLOUR_RGB('MAS-253 Metallic Sheet - Hydraulic Foot Pump Body', 0.66274510, 0.83137255, 0.94901961) ;
#19066 = COLOUR_RGB('MAS-253 Metallic Sheet - Foot Pump Pedal', 0.31764706, 0.68627451, 0.89019608) ;
#19067 = COLOUR_RGB('MAS-253 Metallic Sheet - Push Handle (chrome tube)', 0.40784314, 0.44705882, 0.49803922) ;
#19068 = COLOUR_RGB('MAS-253 Metallic Sheet - Lowering Release Lever', 0.72549020, 0.75294118, 0.79215686) ;
#19069 = COLOUR_RGB(
'MAS-253 Metallic Sheet - Pivot Pin D4 x 11.4 with E-Clip Groove', 0.08235294, 0.09019608, 0.10196078) ;
#19070 = COLOUR_RGB(
'MAS-253 Metallic Sheet - DIN 6799 - 3.2 Retaining Washer (E-Clip)', 0.09019608, 0.27058824, 0.51372549) ;
#19071 = COLOUR_RGB('MAS-253 Metallic Sheet - Track Roller D8 with Stud', 0.66274510, 0.83137255, 0.94901961) ;
#19072 = COLOUR_RGB('MAS-253 Metallic Sheet - ISO 4762 - M2 x 6 - 12.9', 0.31764706, 0.68627451, 0.89019608) ;
#19073 = COLOUR_RGB('MAS-253 Metallic Sheet - Swivel Caster Yoke 4 in', 0.40784314, 0.44705882, 0.49803922) ;
#19074 = COLOUR_RGB('MAS-253 Metallic Sheet - Rigid Caster Yoke 4 in', 0.72549020, 0.75294118, 0.79215686) ;
#19075 = COLOUR_RGB('MAS-253 Metallic Sheet - Caster Wheel 4 in Rubber', 0.08235294, 0.09019608, 0.10196078) ;
ENDSEC;
END-ISO-10303-21;
